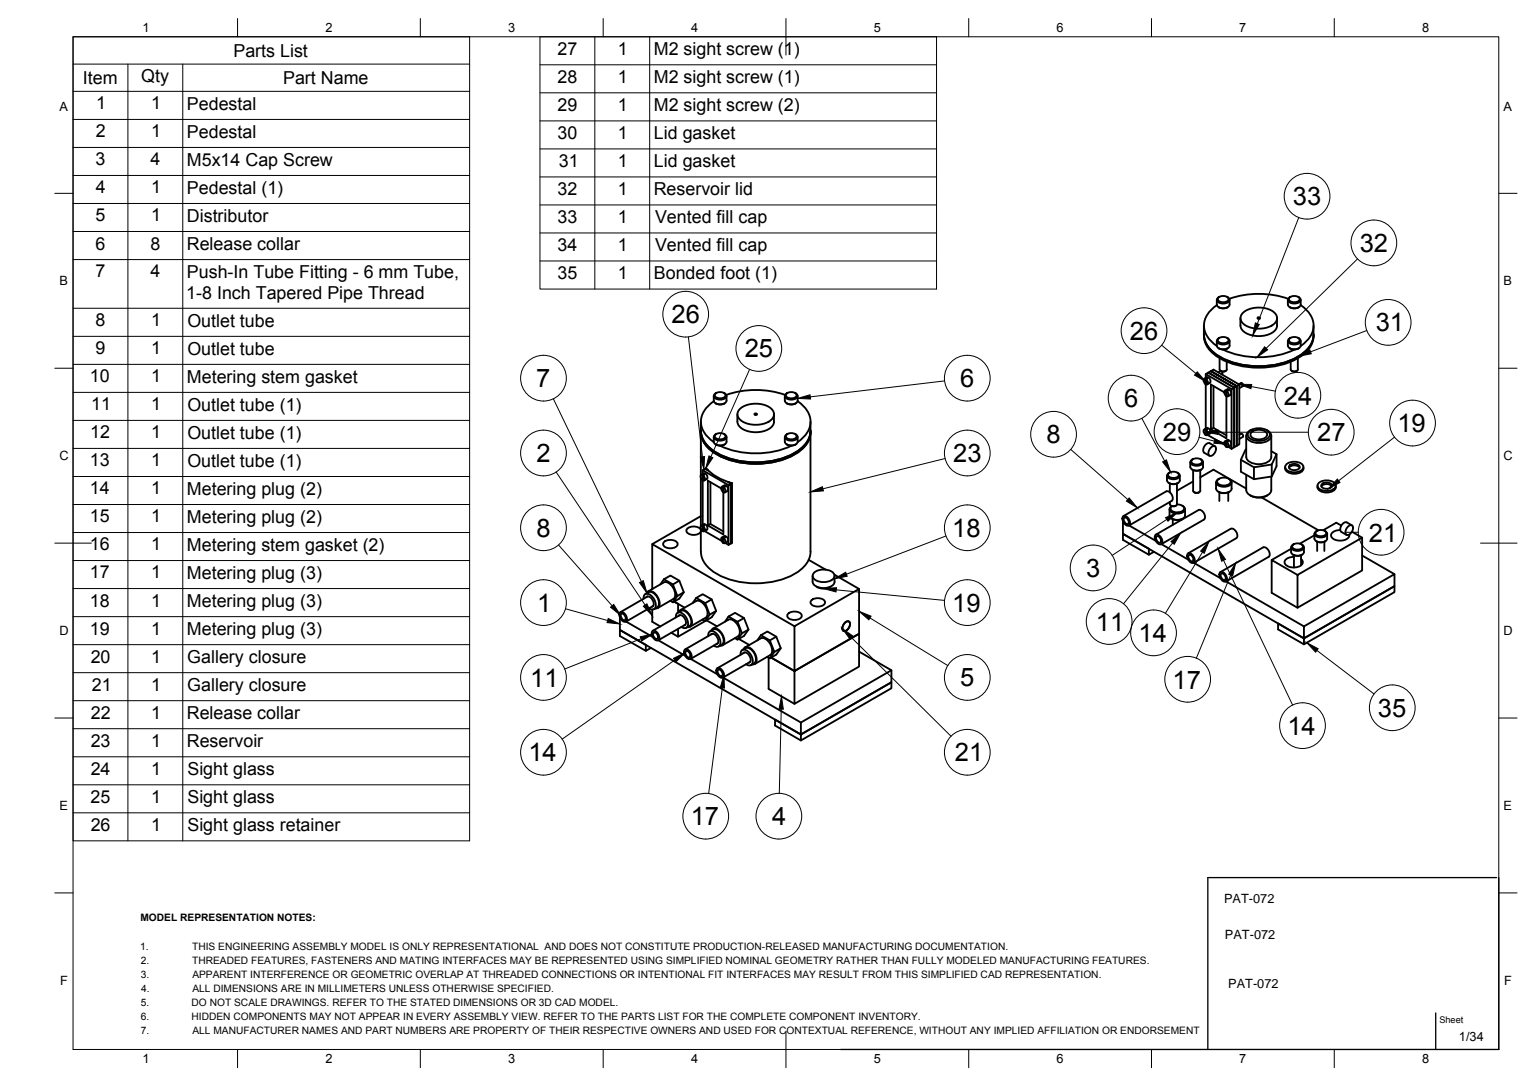
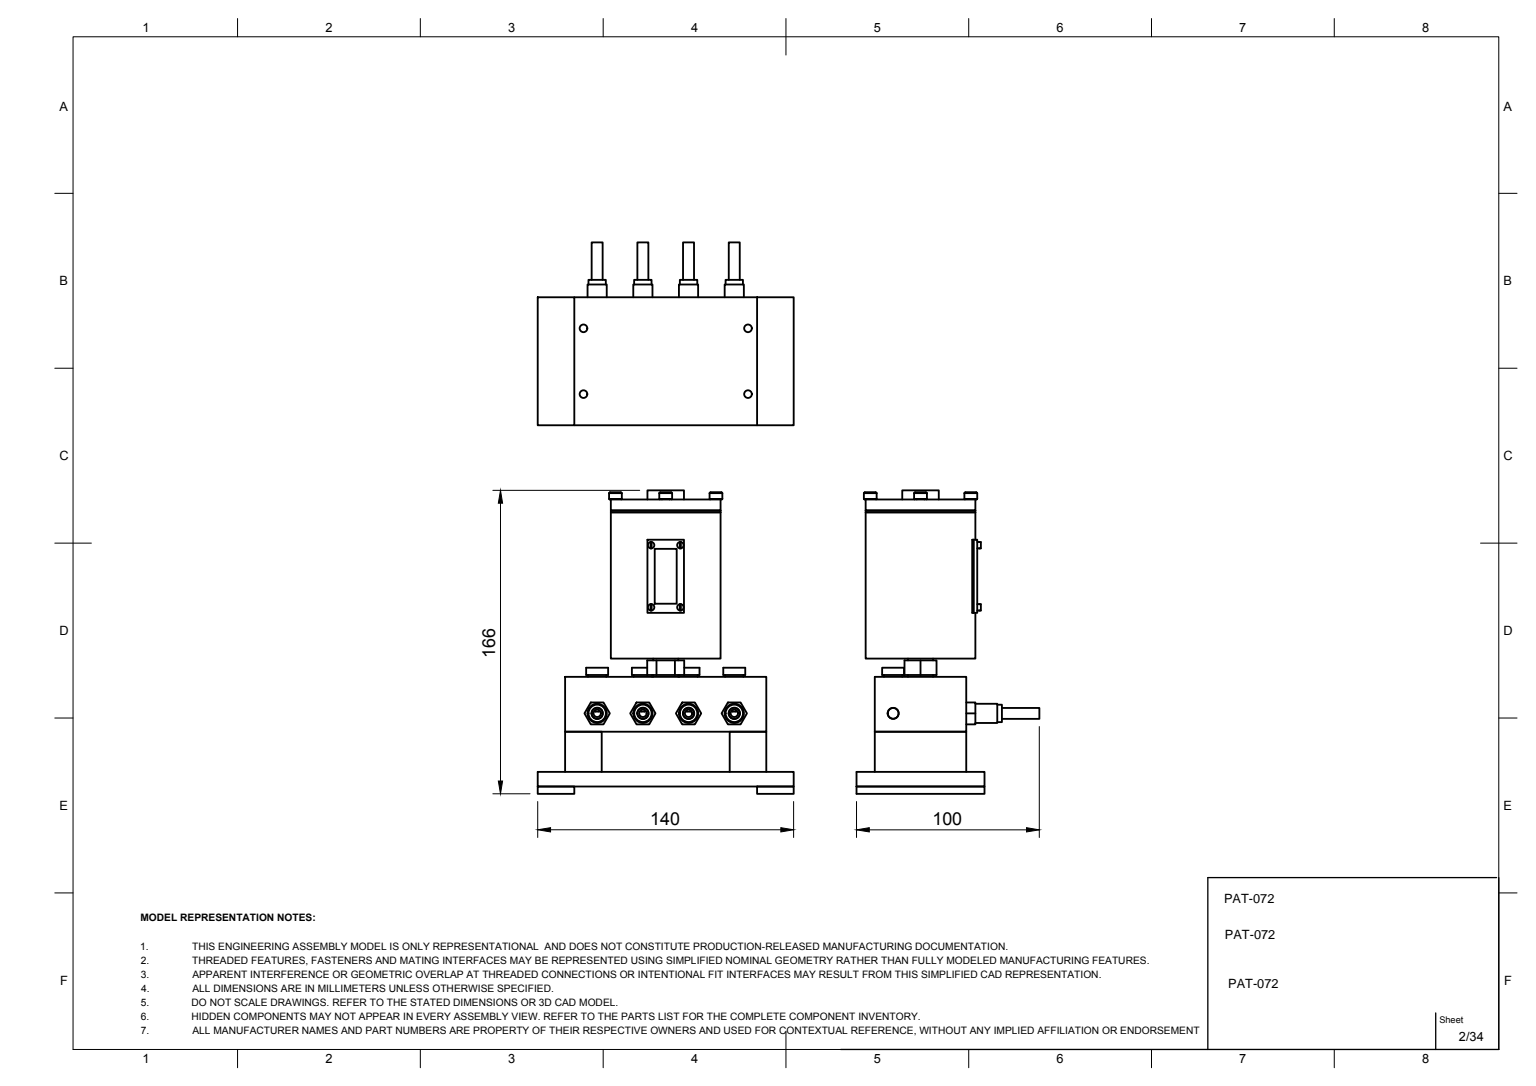
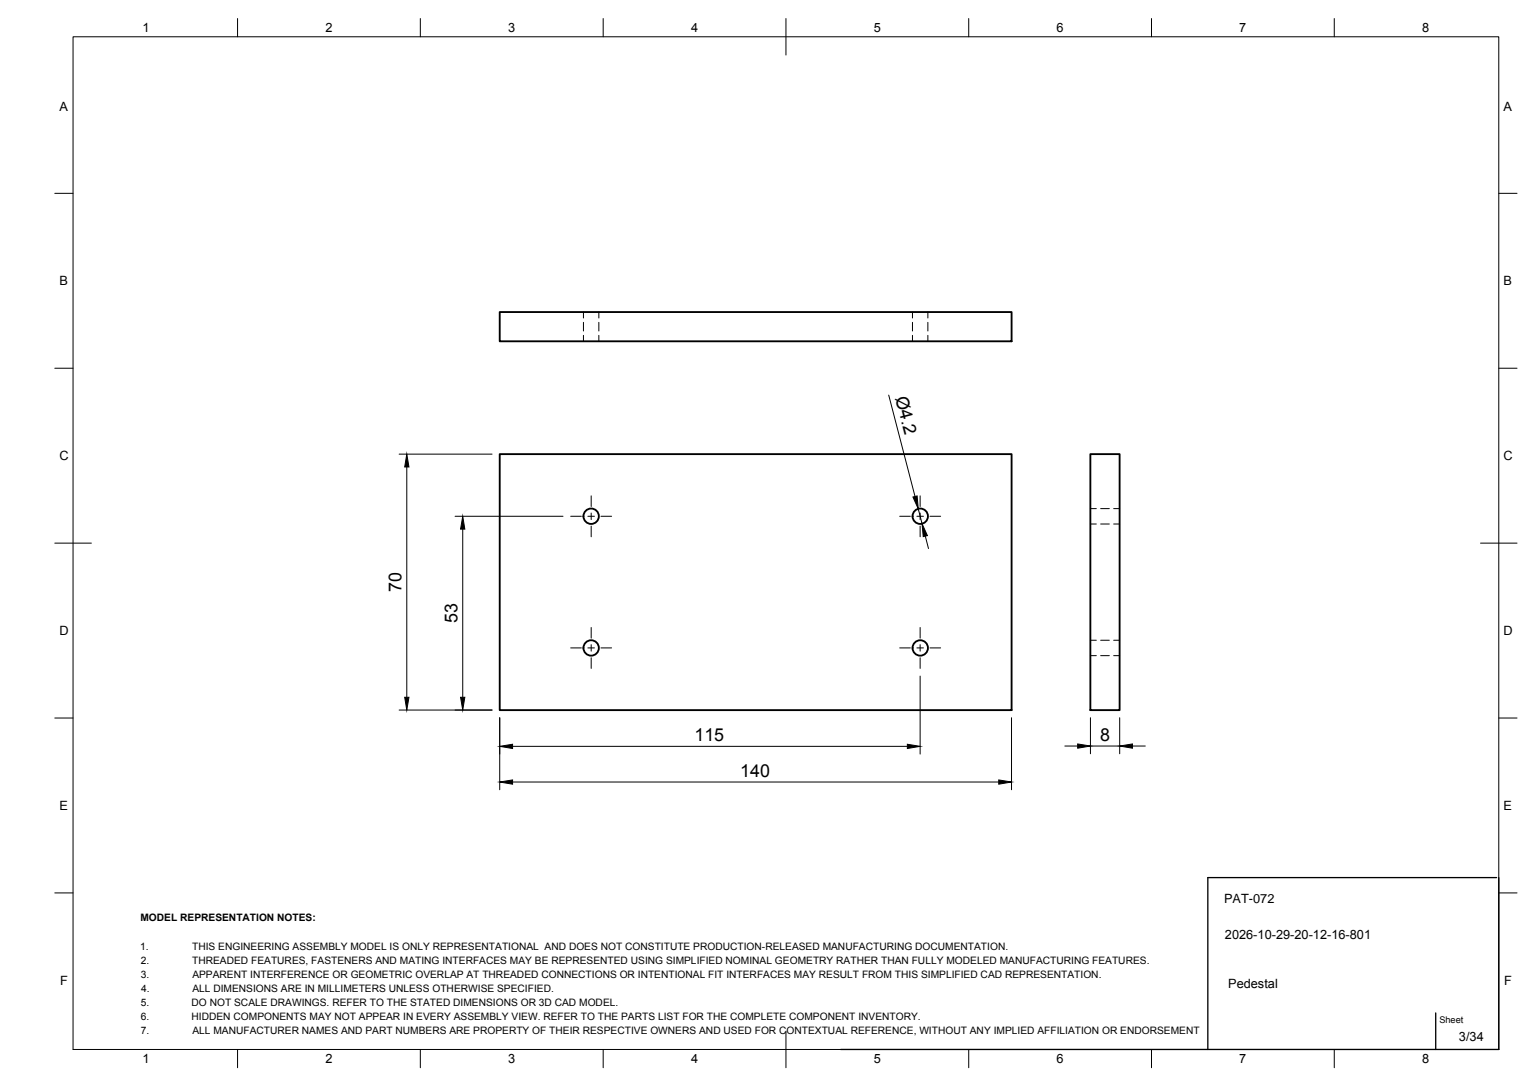
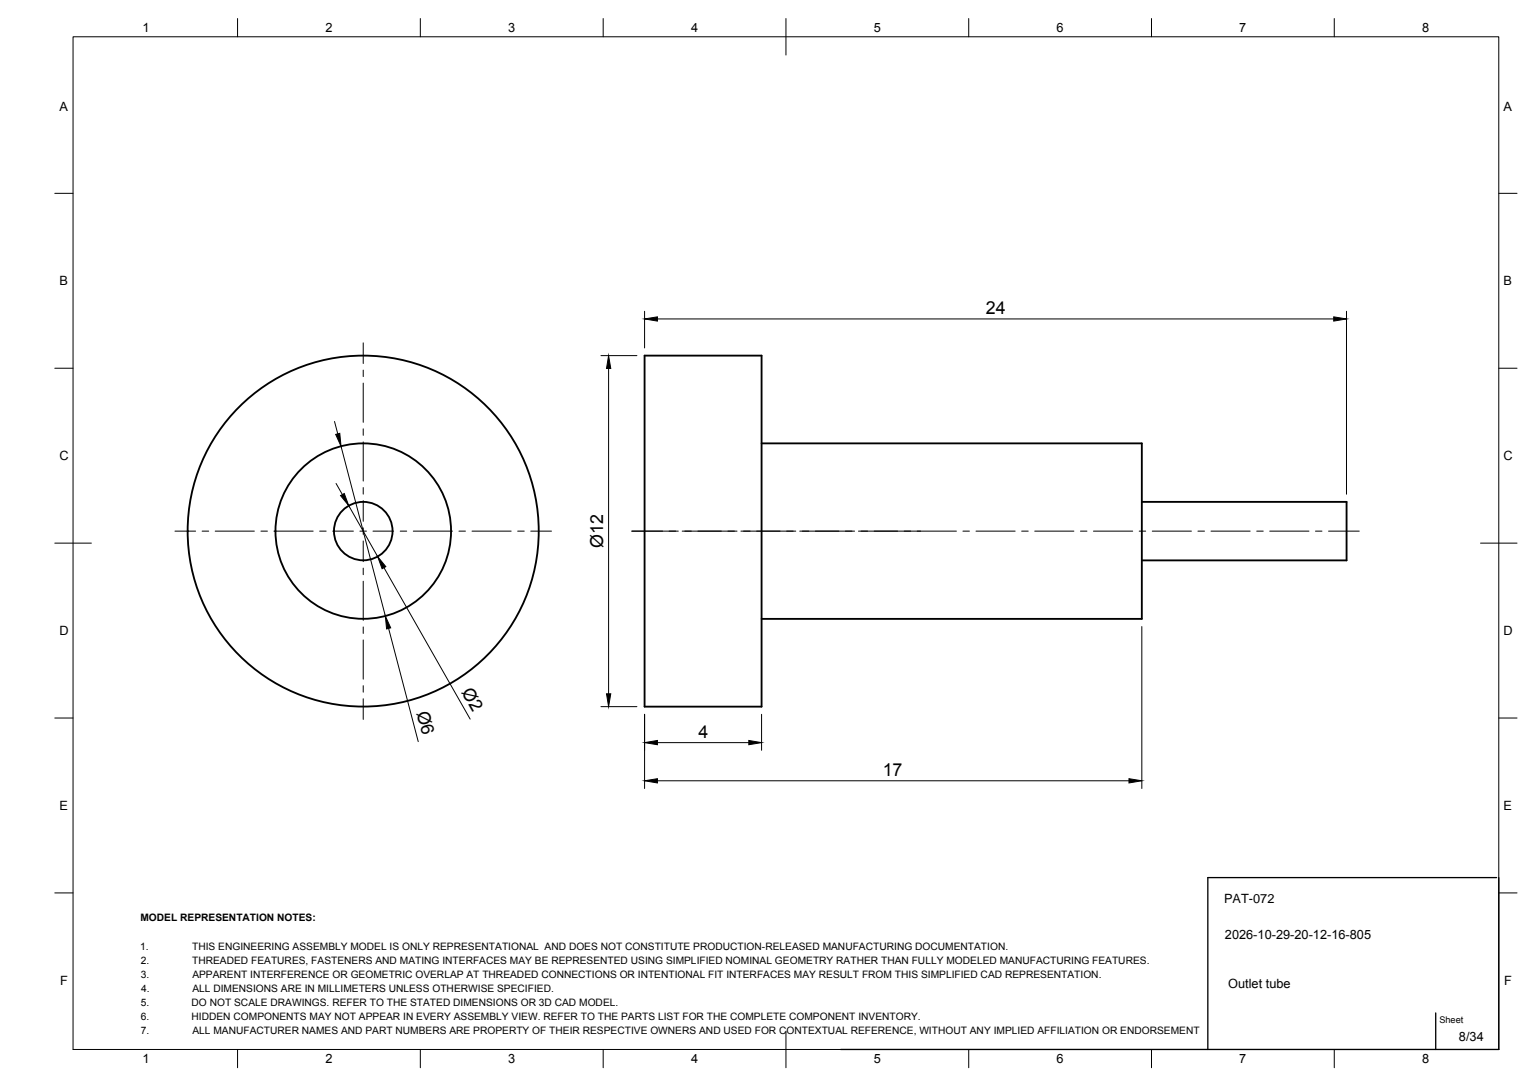
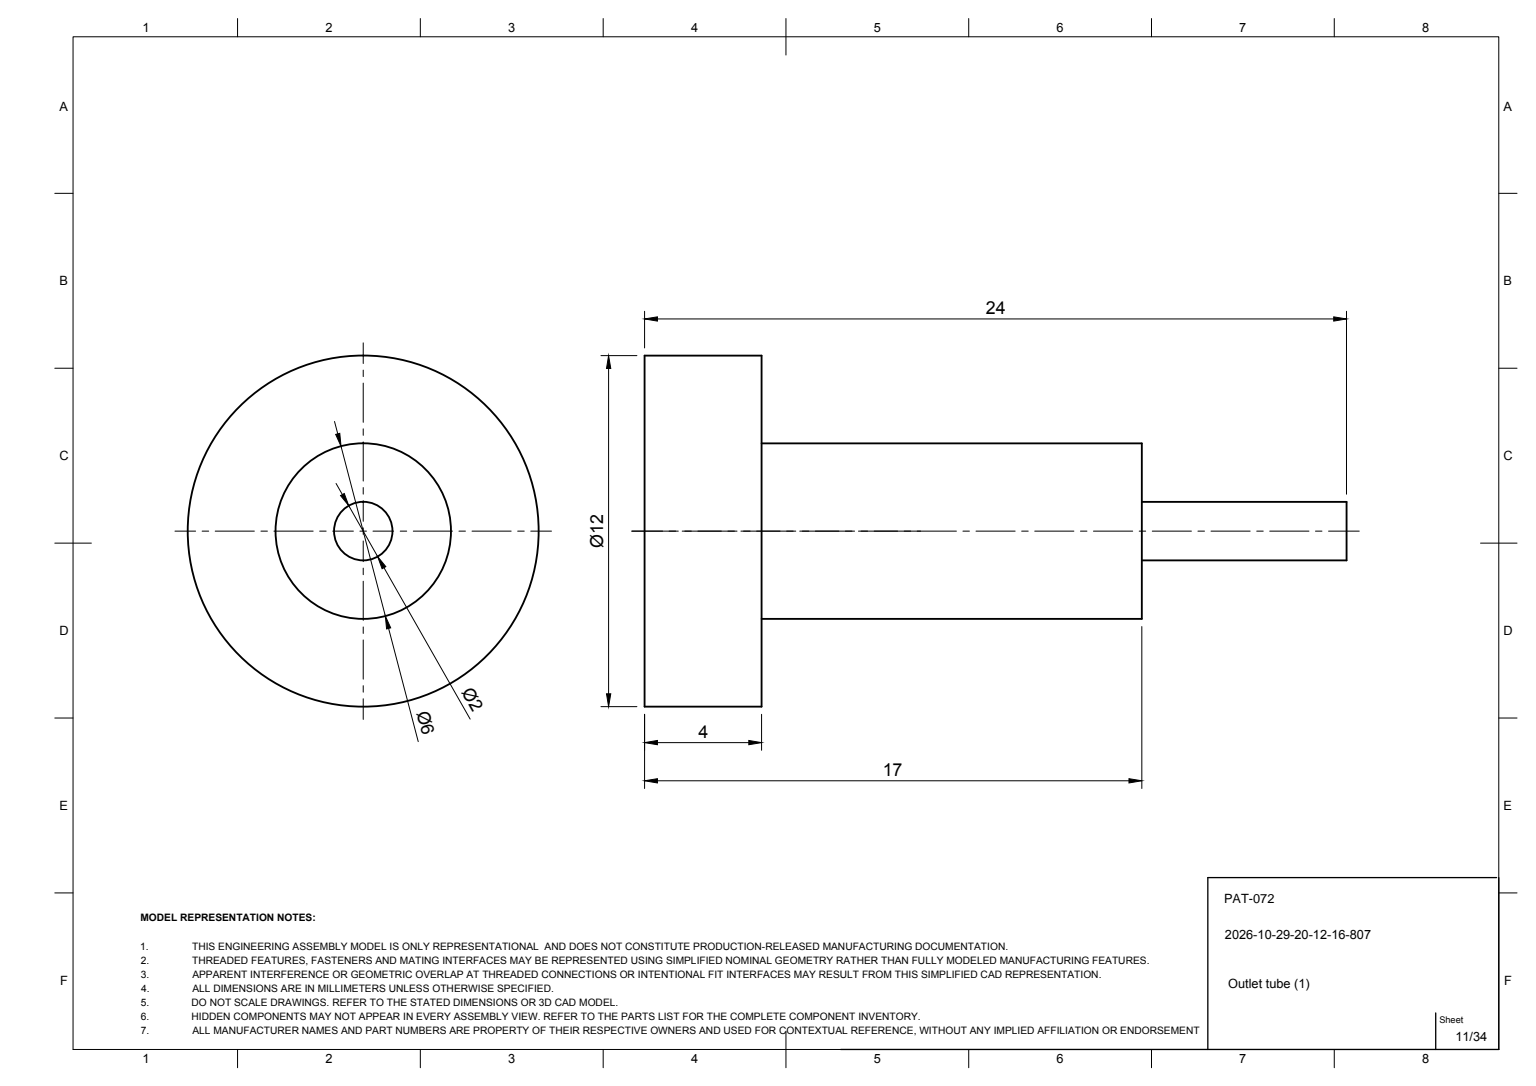
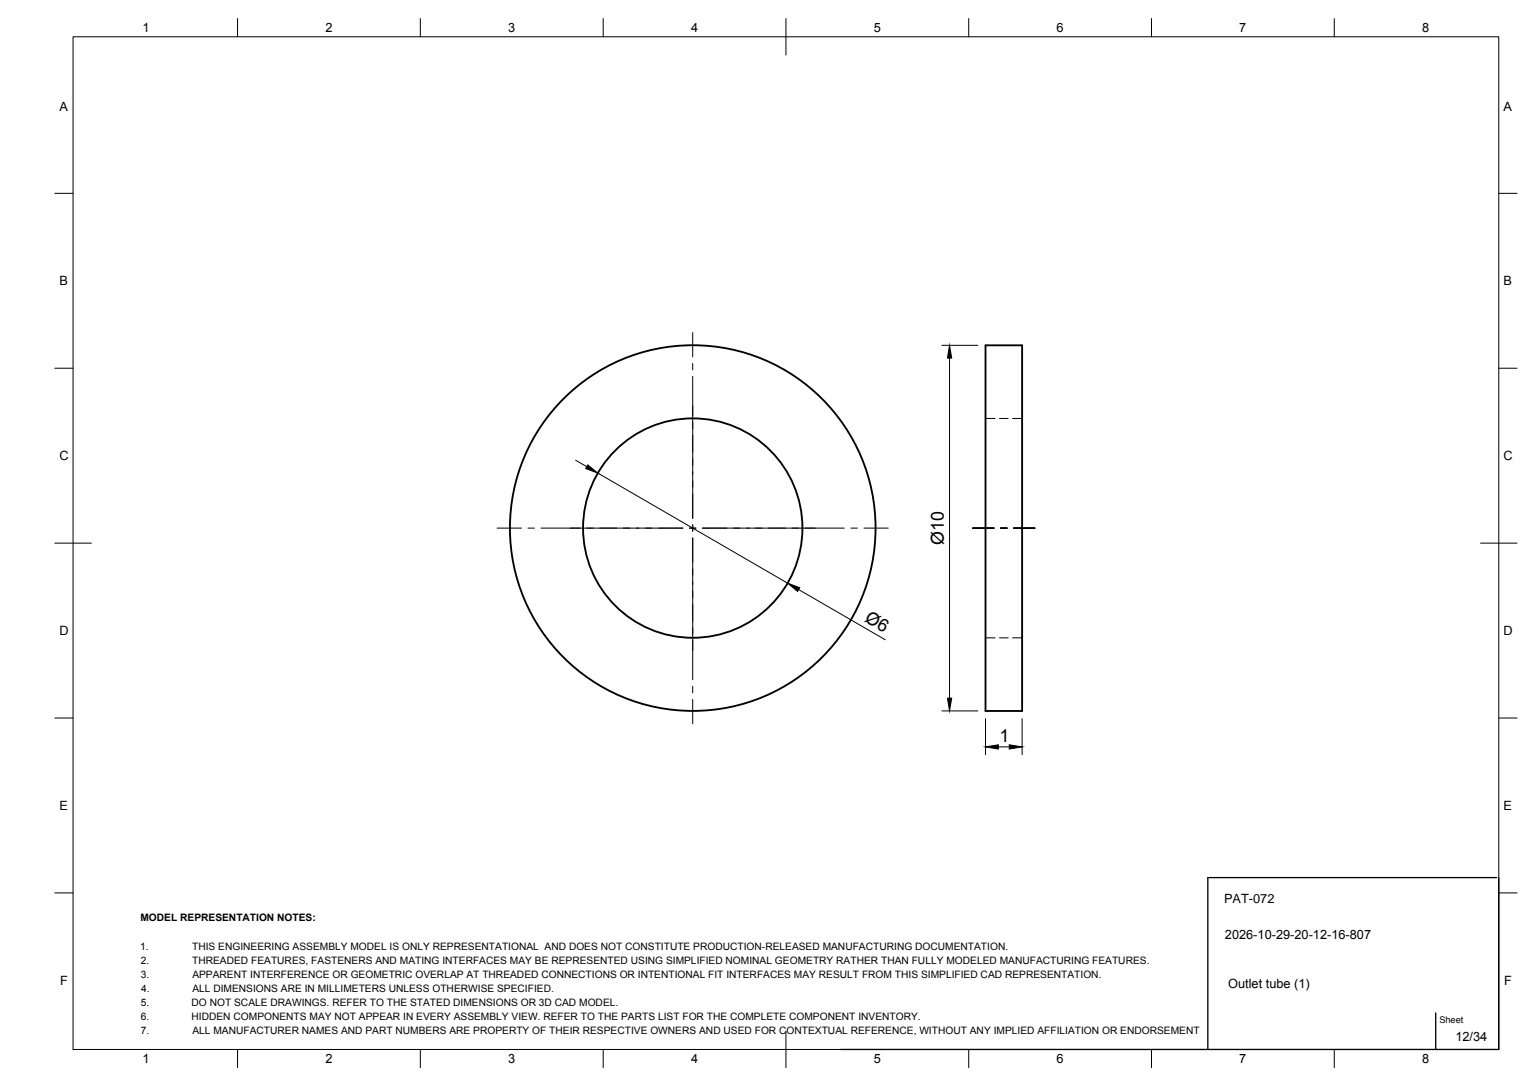
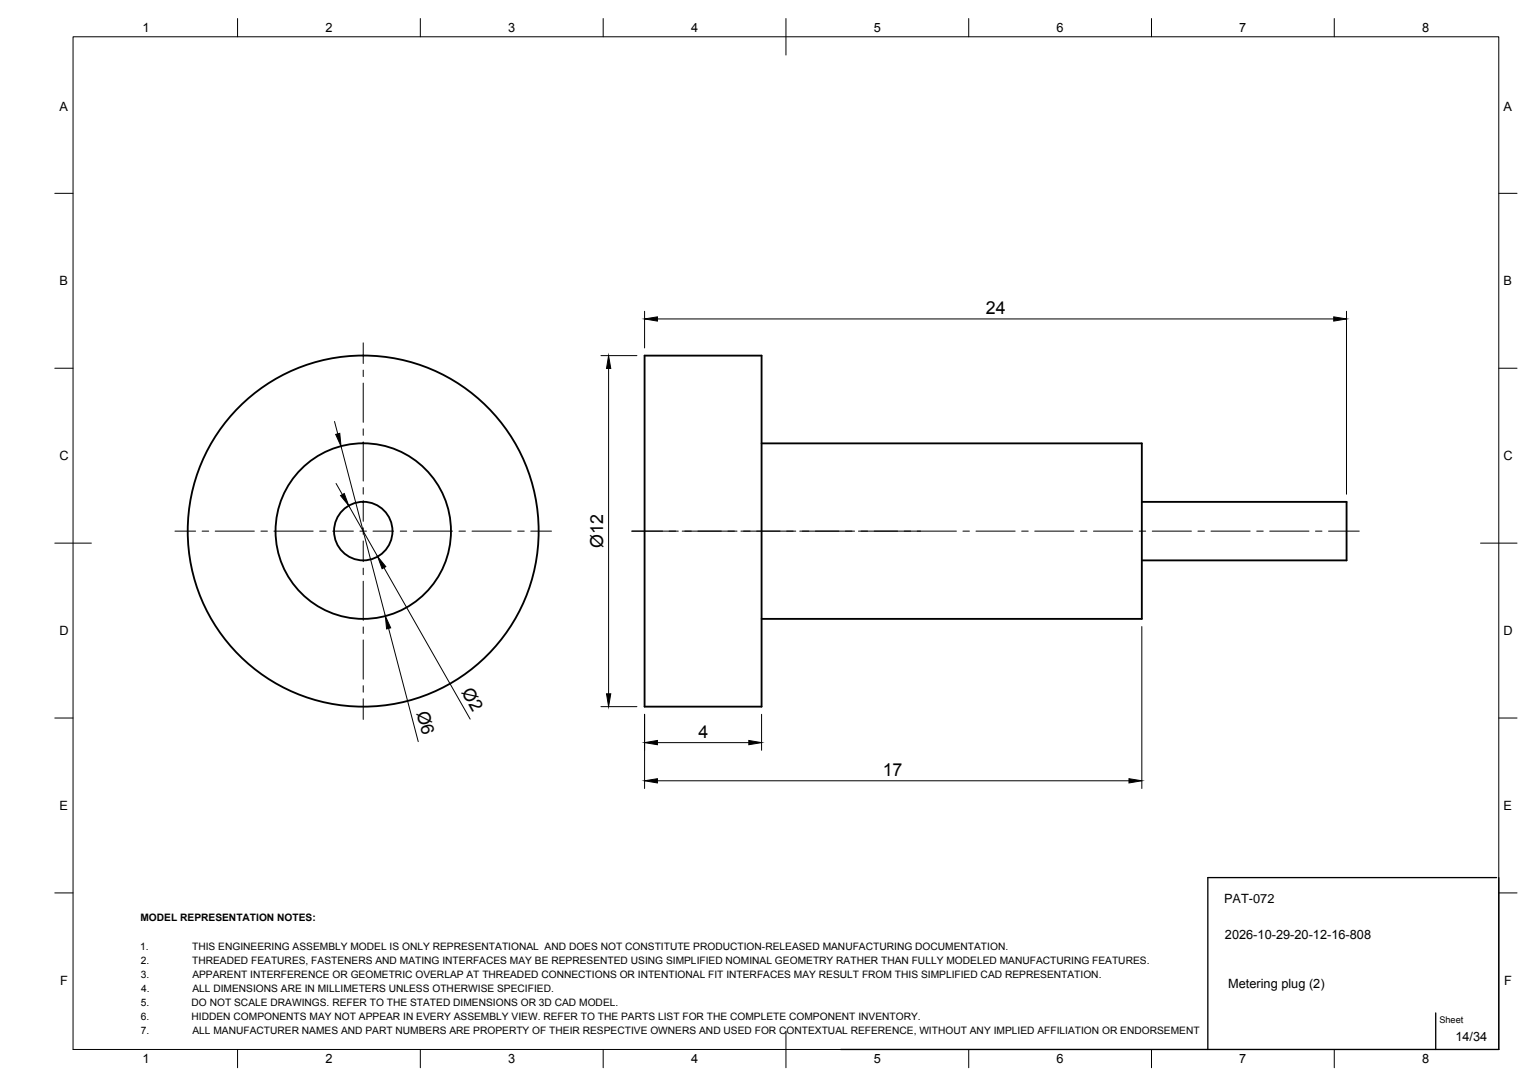
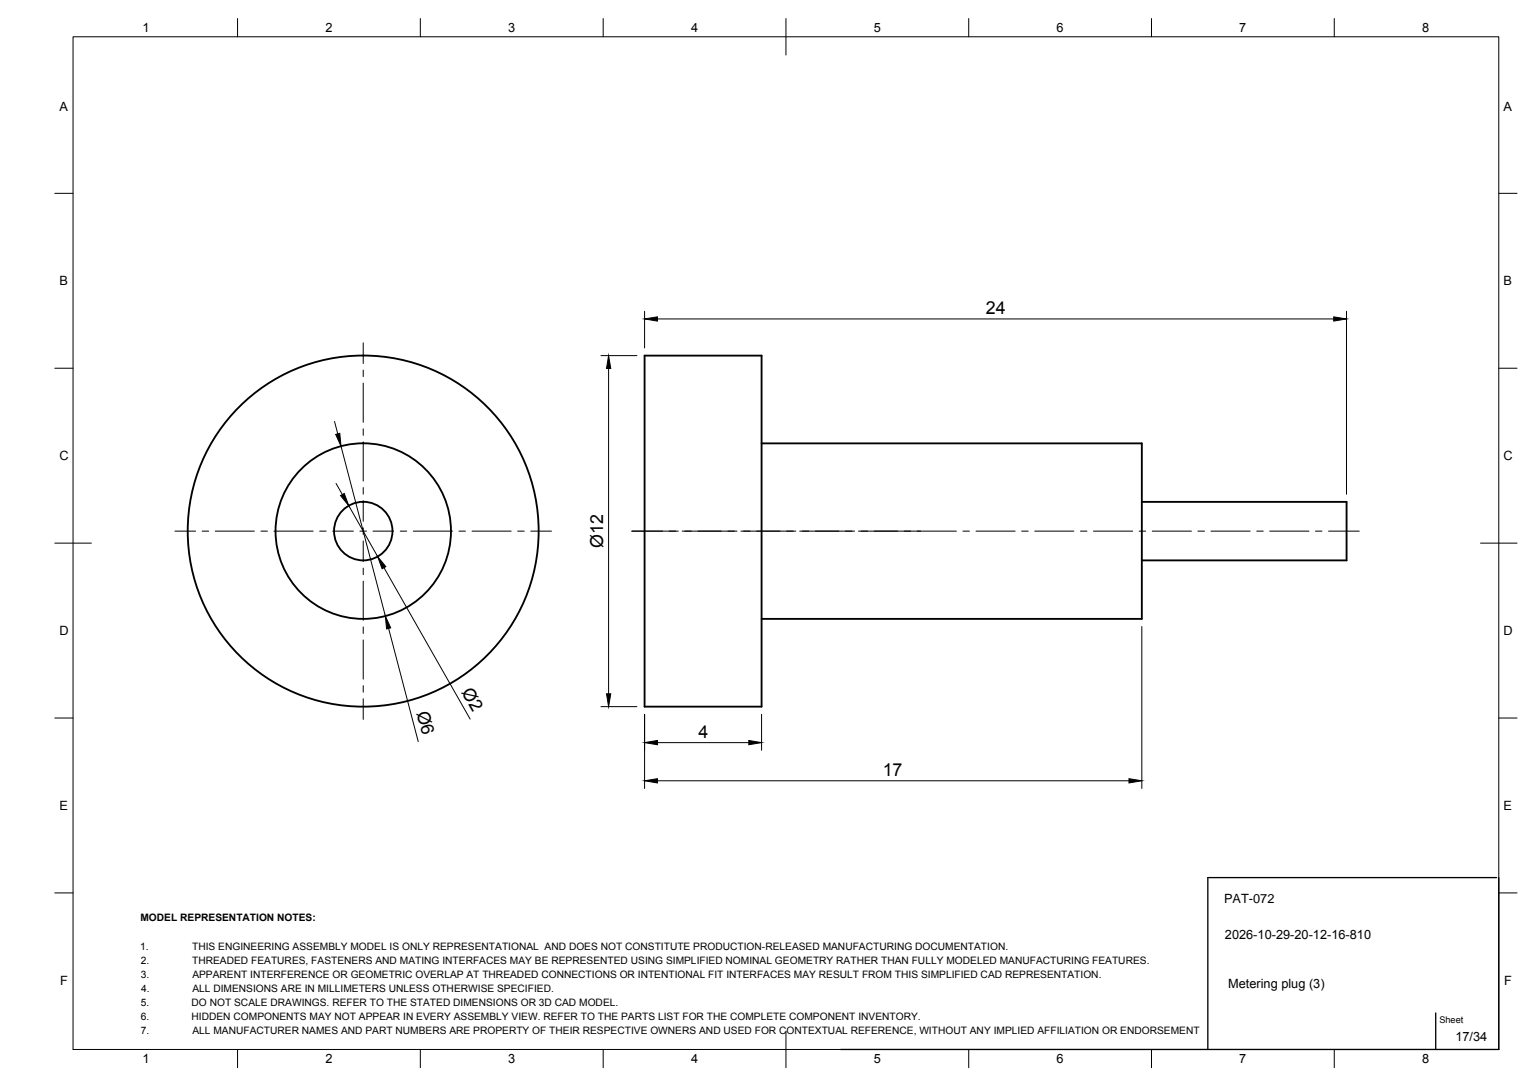
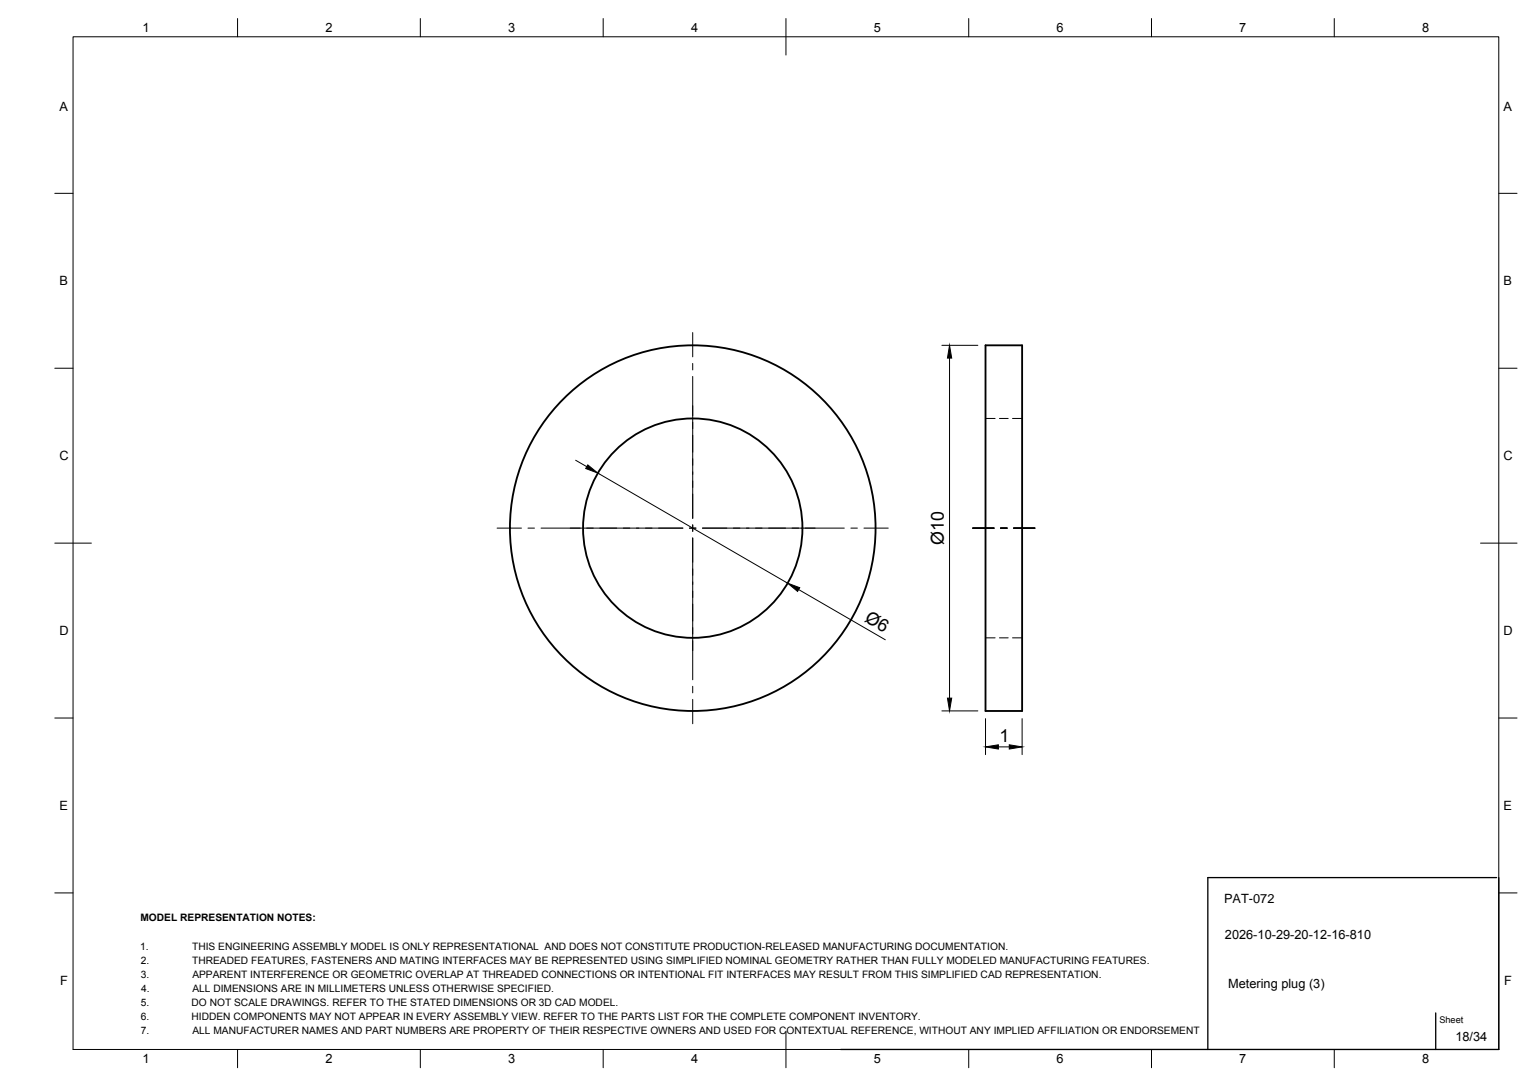
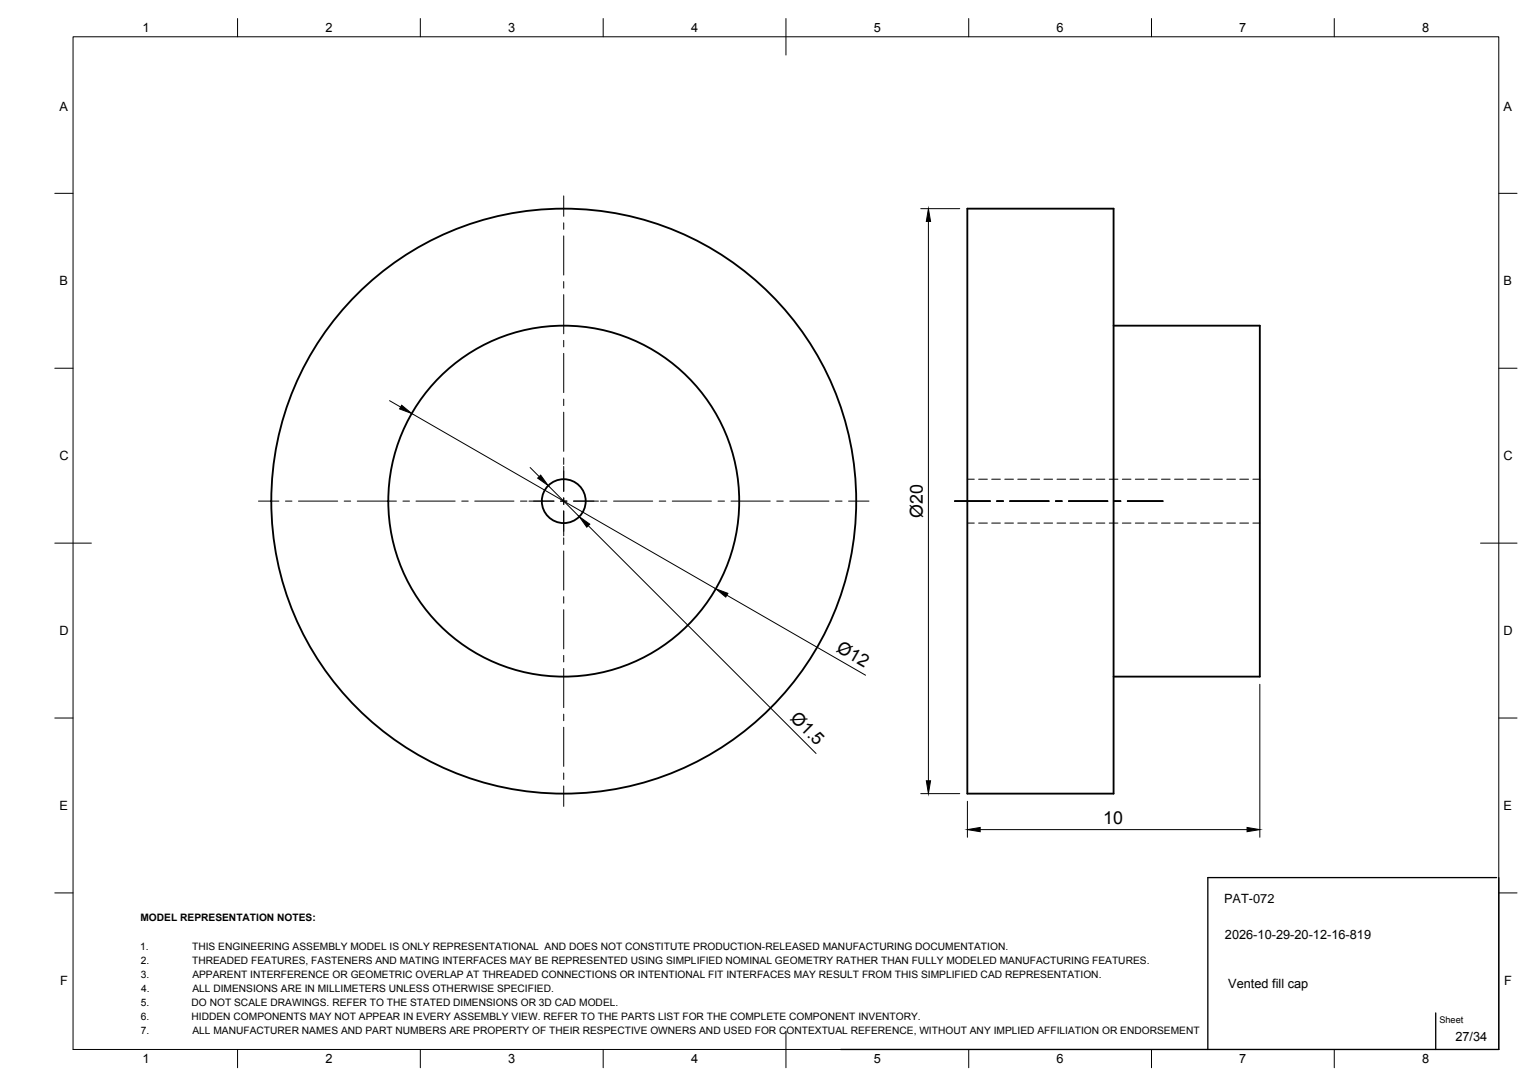
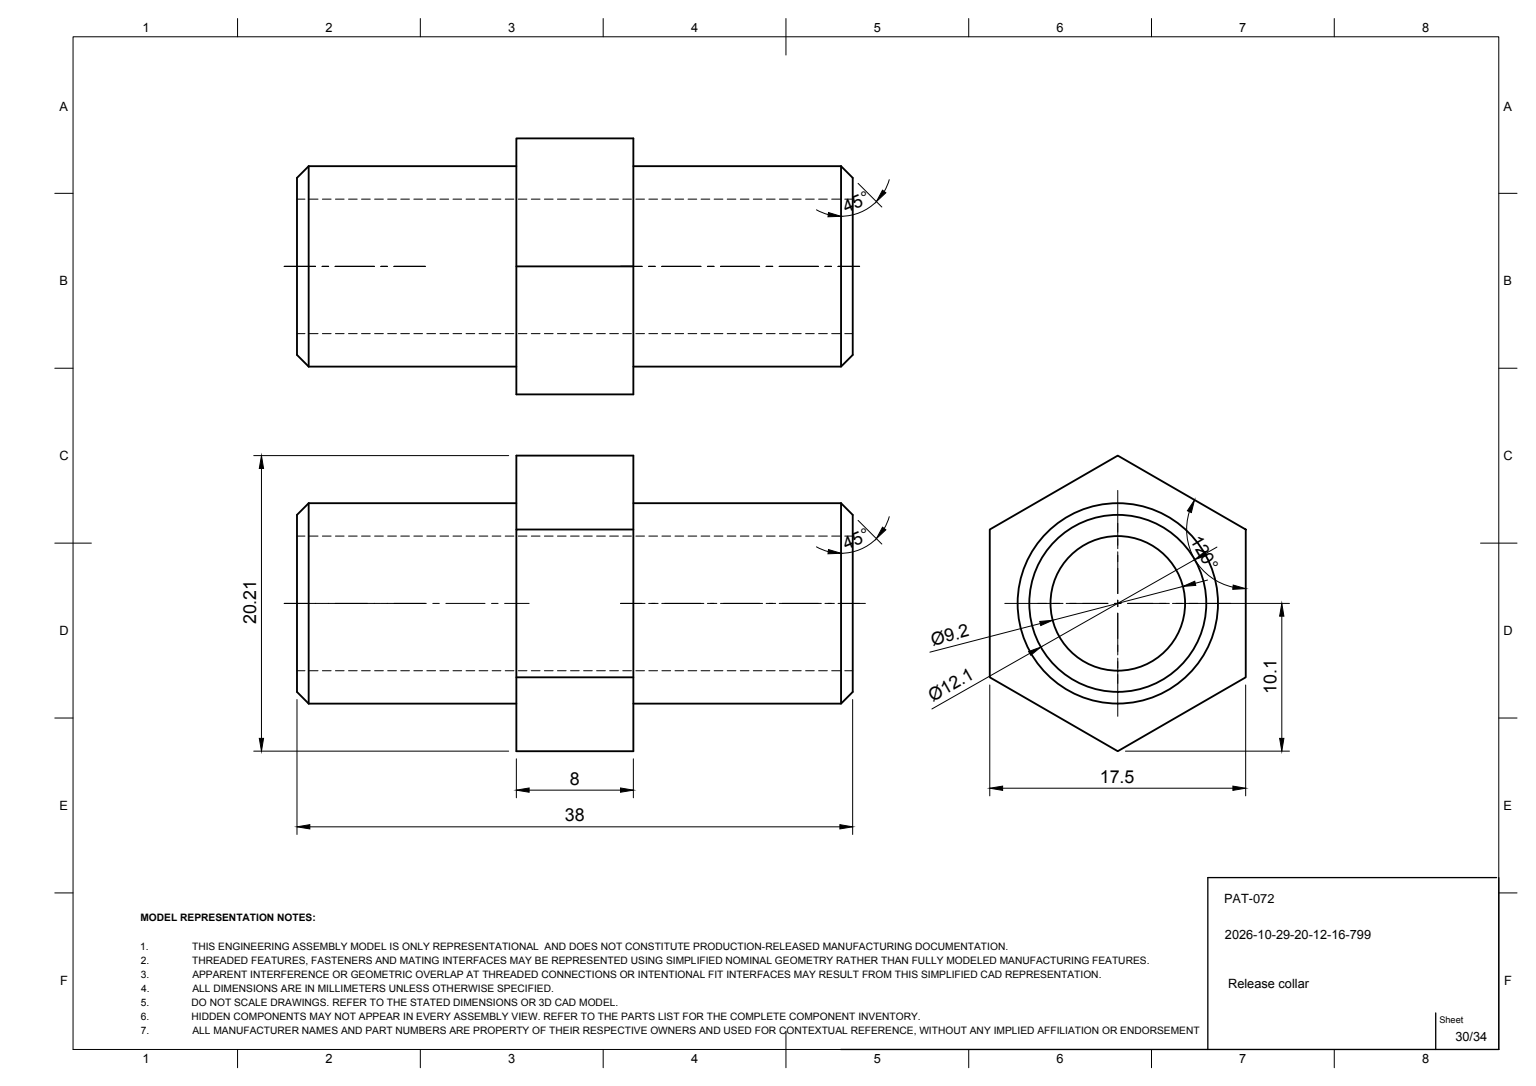
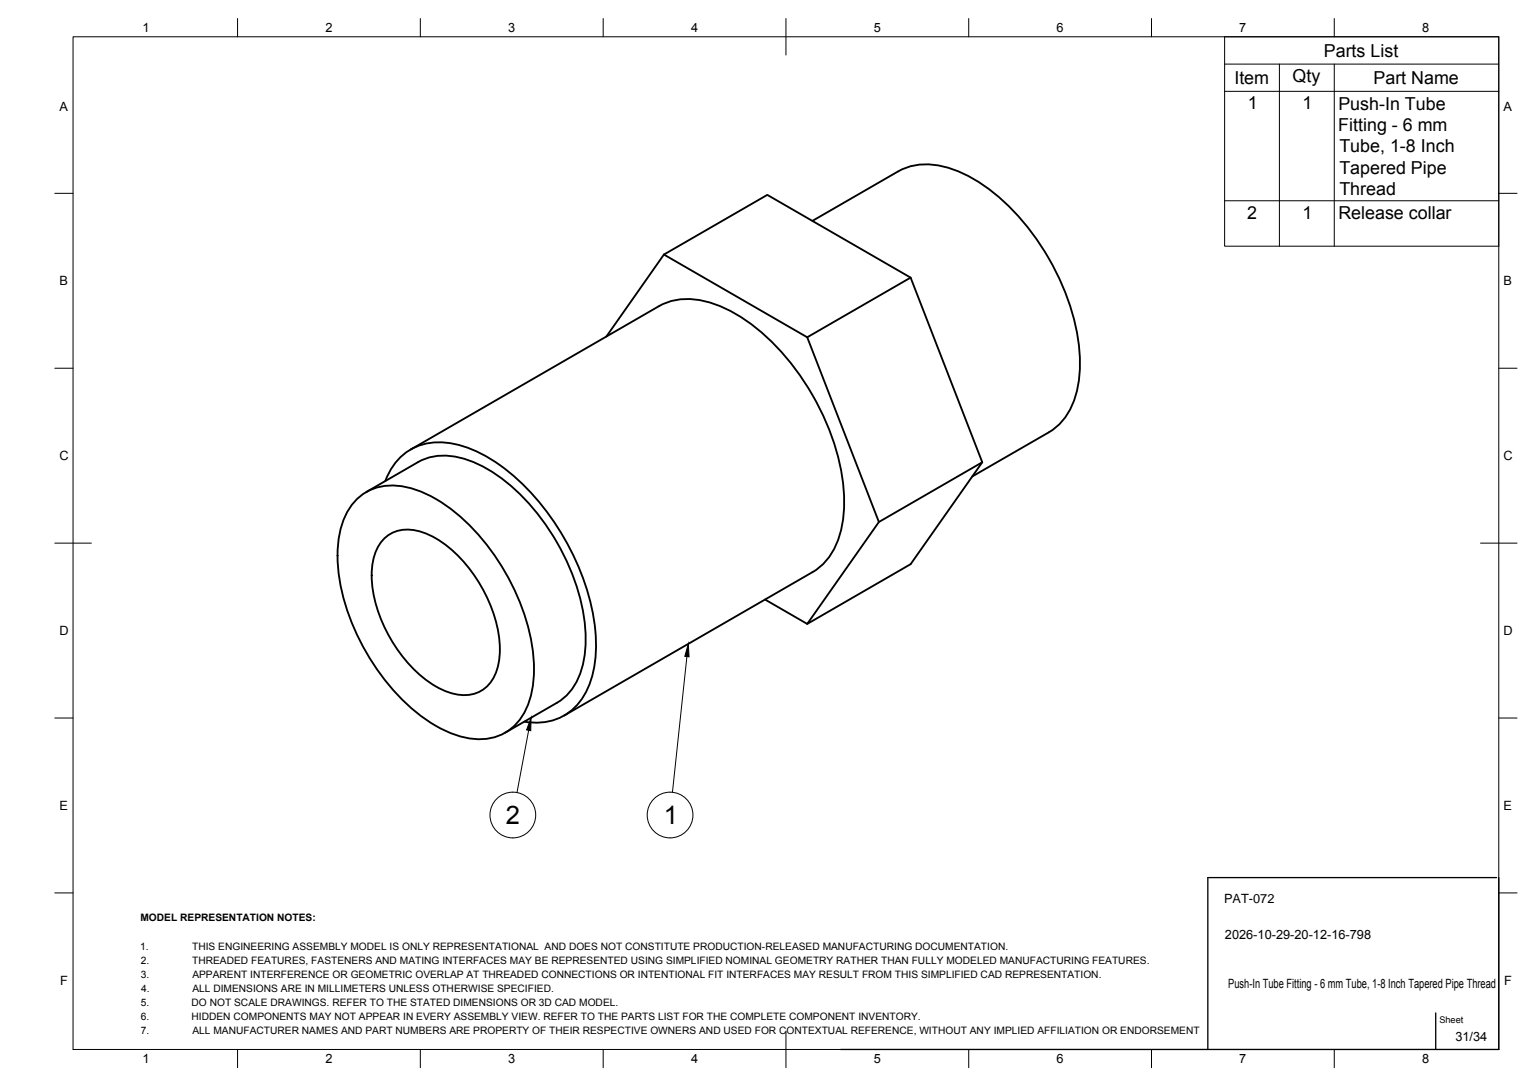
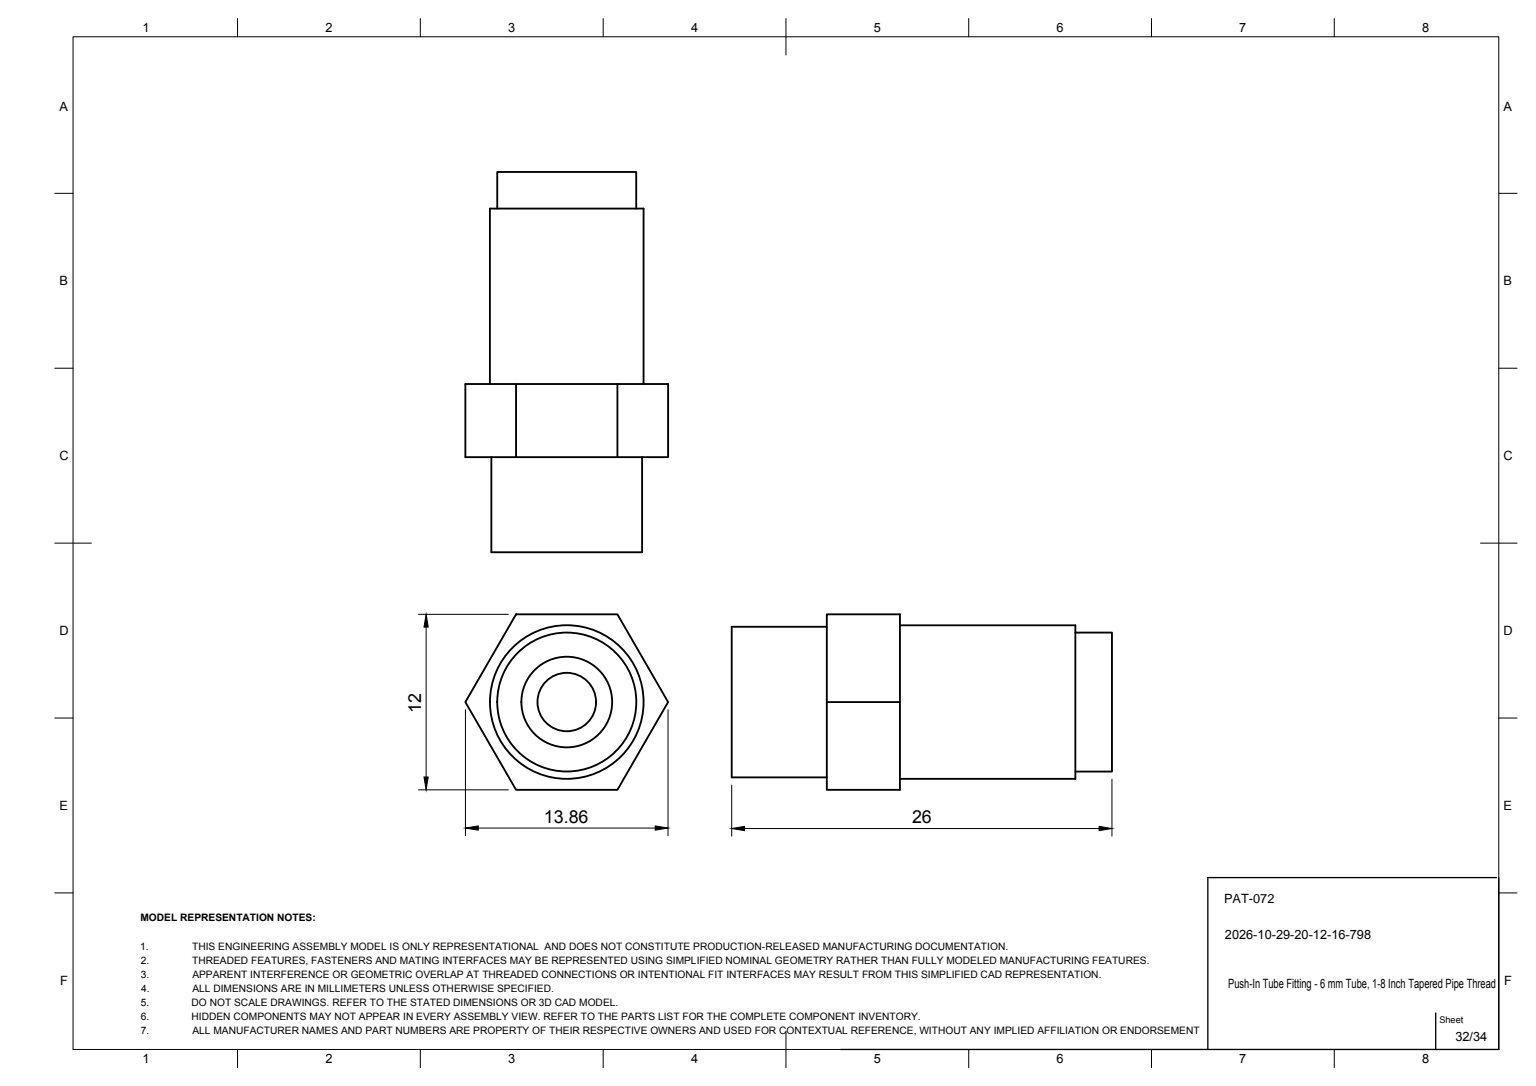
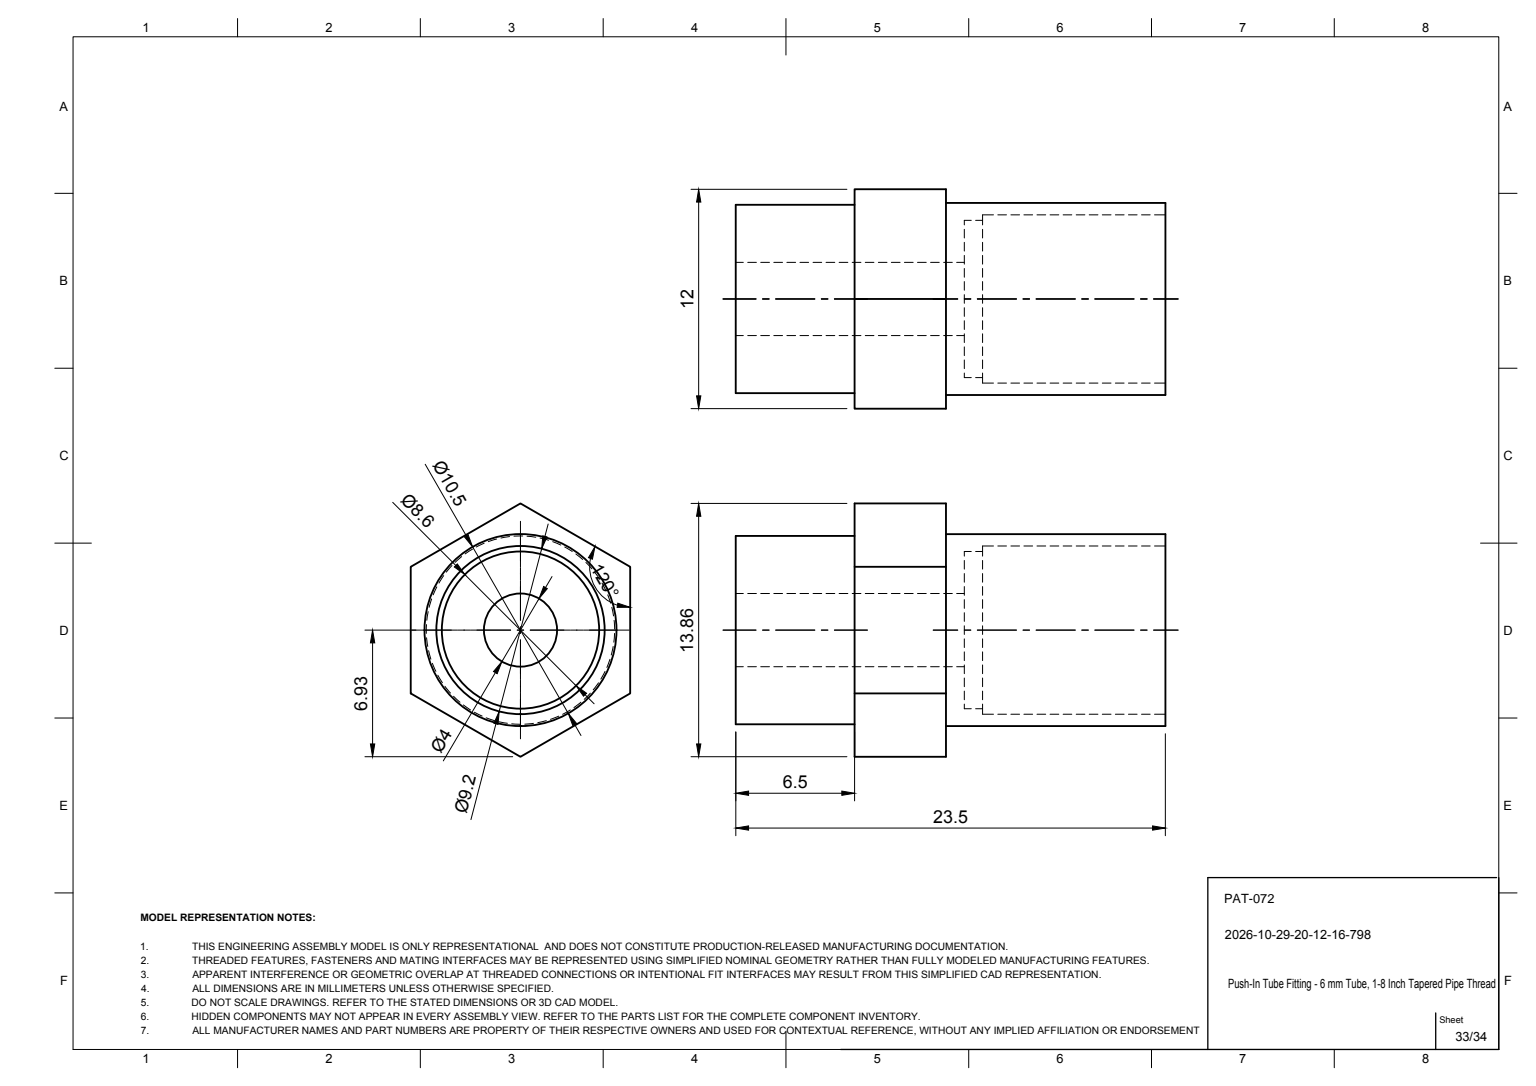
ISO-10303-21;
HEADER;
/* Generated by software containing ST-Developer
 * from STEP Tools, Inc. (www.steptools.com) 
 */

FILE_DESCRIPTION(
/* description */ ('PAT-072'),
/* implementation_level */ '2;1');

FILE_NAME(
/* name */ 'PAT-072',
/* time_stamp */ '2026-10-29T20:11:56-07:00',
/* author */ (''),
/* organization */ (''),
/* preprocessor_version */ 'ST-DEVELOPER v20.2',
/* originating_system */ 'Autodesk Translation Framework v15.17.0.0',
/* authorisation */ '');

FILE_SCHEMA (('AUTOMOTIVE_DESIGN { 1 0 10303 214 3 1 1 }'));
ENDSEC;

DATA;
#10=MECHANICAL_DESIGN_GEOMETRIC_PRESENTATION_REPRESENTATION('',(#332,#333,
#334,#335,#336,#337,#338,#339,#340,#341,#342,#343,#344,#345,#346,#347,#348,
#349,#350,#351,#352,#353,#354,#355,#356,#357,#358,#359,#360,#361,#362,#363,
#364,#365,#366,#367),#11432);
#11=ITEM_DEFINED_TRANSFORMATION($,$,#7118,#7159);
#12=ITEM_DEFINED_TRANSFORMATION($,$,#7146,#7160);
#13=ITEM_DEFINED_TRANSFORMATION($,$,#6503,#7211);
#14=ITEM_DEFINED_TRANSFORMATION($,$,#6522,#7212);
#15=ITEM_DEFINED_TRANSFORMATION($,$,#6547,#7213);
#16=ITEM_DEFINED_TRANSFORMATION($,$,#6572,#7214);
#17=ITEM_DEFINED_TRANSFORMATION($,$,#6692,#7215);
#18=ITEM_DEFINED_TRANSFORMATION($,$,#6701,#7216);
#19=ITEM_DEFINED_TRANSFORMATION($,$,#6715,#7217);
#20=ITEM_DEFINED_TRANSFORMATION($,$,#6724,#7218);
#21=ITEM_DEFINED_TRANSFORMATION($,$,#6733,#7219);
#22=ITEM_DEFINED_TRANSFORMATION($,$,#6747,#7220);
#23=ITEM_DEFINED_TRANSFORMATION($,$,#6756,#7221);
#24=ITEM_DEFINED_TRANSFORMATION($,$,#6765,#7222);
#25=ITEM_DEFINED_TRANSFORMATION($,$,#6779,#7223);
#26=ITEM_DEFINED_TRANSFORMATION($,$,#6788,#7224);
#27=ITEM_DEFINED_TRANSFORMATION($,$,#6797,#7225);
#28=ITEM_DEFINED_TRANSFORMATION($,$,#6811,#7226);
#29=ITEM_DEFINED_TRANSFORMATION($,$,#6820,#7227);
#30=ITEM_DEFINED_TRANSFORMATION($,$,#6826,#7228);
#31=ITEM_DEFINED_TRANSFORMATION($,$,#6832,#7229);
#32=ITEM_DEFINED_TRANSFORMATION($,$,#6887,#7230);
#33=ITEM_DEFINED_TRANSFORMATION($,$,#6910,#7231);
#34=ITEM_DEFINED_TRANSFORMATION($,$,#6929,#7232);
#35=ITEM_DEFINED_TRANSFORMATION($,$,#6952,#7233);
#36=ITEM_DEFINED_TRANSFORMATION($,$,#6970,#7234);
#37=ITEM_DEFINED_TRANSFORMATION($,$,#6988,#7235);
#38=ITEM_DEFINED_TRANSFORMATION($,$,#7006,#7236);
#39=ITEM_DEFINED_TRANSFORMATION($,$,#7024,#7237);
#40=ITEM_DEFINED_TRANSFORMATION($,$,#7045,#7238);
#41=ITEM_DEFINED_TRANSFORMATION($,$,#7066,#7239);
#42=ITEM_DEFINED_TRANSFORMATION($,$,#7079,#7240);
#43=ITEM_DEFINED_TRANSFORMATION($,$,#7086,#7241);
#44=ITEM_DEFINED_TRANSFORMATION($,$,#7093,#7242);
#45=ITEM_DEFINED_TRANSFORMATION($,$,#7093,#7243);
#46=ITEM_DEFINED_TRANSFORMATION($,$,#7093,#7244);
#47=ITEM_DEFINED_TRANSFORMATION($,$,#7093,#7245);
#48=ITEM_DEFINED_TRANSFORMATION($,$,#7185,#7246);
#49=ITEM_DEFINED_TRANSFORMATION($,$,#7185,#7247);
#50=ITEM_DEFINED_TRANSFORMATION($,$,#7185,#7248);
#51=ITEM_DEFINED_TRANSFORMATION($,$,#7185,#7249);
#52=ITEM_DEFINED_TRANSFORMATION($,$,#7117,#7250);
#53=ITEM_DEFINED_TRANSFORMATION($,$,#7117,#7251);
#54=ITEM_DEFINED_TRANSFORMATION($,$,#7117,#7252);
#55=ITEM_DEFINED_TRANSFORMATION($,$,#7117,#7253);
#56=ITEM_DEFINED_TRANSFORMATION($,$,#7161,#7254);
#57=ITEM_DEFINED_TRANSFORMATION($,$,#7185,#7255);
#58=ITEM_DEFINED_TRANSFORMATION($,$,#7185,#7256);
#59=ITEM_DEFINED_TRANSFORMATION($,$,#7185,#7257);
#60=ITEM_DEFINED_TRANSFORMATION($,$,#7185,#7258);
#61=(
REPRESENTATION_RELATIONSHIP($,$,#11597,#11596)
REPRESENTATION_RELATIONSHIP_WITH_TRANSFORMATION(#11)
SHAPE_REPRESENTATION_RELATIONSHIP()
);
#62=(
REPRESENTATION_RELATIONSHIP($,$,#11598,#11596)
REPRESENTATION_RELATIONSHIP_WITH_TRANSFORMATION(#12)
SHAPE_REPRESENTATION_RELATIONSHIP()
);
#63=(
REPRESENTATION_RELATIONSHIP($,$,#11564,#11563)
REPRESENTATION_RELATIONSHIP_WITH_TRANSFORMATION(#13)
SHAPE_REPRESENTATION_RELATIONSHIP()
);
#64=(
REPRESENTATION_RELATIONSHIP($,$,#11565,#11563)
REPRESENTATION_RELATIONSHIP_WITH_TRANSFORMATION(#14)
SHAPE_REPRESENTATION_RELATIONSHIP()
);
#65=(
REPRESENTATION_RELATIONSHIP($,$,#11566,#11563)
REPRESENTATION_RELATIONSHIP_WITH_TRANSFORMATION(#15)
SHAPE_REPRESENTATION_RELATIONSHIP()
);
#66=(
REPRESENTATION_RELATIONSHIP($,$,#11567,#11563)
REPRESENTATION_RELATIONSHIP_WITH_TRANSFORMATION(#16)
SHAPE_REPRESENTATION_RELATIONSHIP()
);
#67=(
REPRESENTATION_RELATIONSHIP($,$,#11568,#11563)
REPRESENTATION_RELATIONSHIP_WITH_TRANSFORMATION(#17)
SHAPE_REPRESENTATION_RELATIONSHIP()
);
#68=(
REPRESENTATION_RELATIONSHIP($,$,#11569,#11563)
REPRESENTATION_RELATIONSHIP_WITH_TRANSFORMATION(#18)
SHAPE_REPRESENTATION_RELATIONSHIP()
);
#69=(
REPRESENTATION_RELATIONSHIP($,$,#11570,#11563)
REPRESENTATION_RELATIONSHIP_WITH_TRANSFORMATION(#19)
SHAPE_REPRESENTATION_RELATIONSHIP()
);
#70=(
REPRESENTATION_RELATIONSHIP($,$,#11571,#11563)
REPRESENTATION_RELATIONSHIP_WITH_TRANSFORMATION(#20)
SHAPE_REPRESENTATION_RELATIONSHIP()
);
#71=(
REPRESENTATION_RELATIONSHIP($,$,#11572,#11563)
REPRESENTATION_RELATIONSHIP_WITH_TRANSFORMATION(#21)
SHAPE_REPRESENTATION_RELATIONSHIP()
);
#72=(
REPRESENTATION_RELATIONSHIP($,$,#11573,#11563)
REPRESENTATION_RELATIONSHIP_WITH_TRANSFORMATION(#22)
SHAPE_REPRESENTATION_RELATIONSHIP()
);
#73=(
REPRESENTATION_RELATIONSHIP($,$,#11574,#11563)
REPRESENTATION_RELATIONSHIP_WITH_TRANSFORMATION(#23)
SHAPE_REPRESENTATION_RELATIONSHIP()
);
#74=(
REPRESENTATION_RELATIONSHIP($,$,#11575,#11563)
REPRESENTATION_RELATIONSHIP_WITH_TRANSFORMATION(#24)
SHAPE_REPRESENTATION_RELATIONSHIP()
);
#75=(
REPRESENTATION_RELATIONSHIP($,$,#11576,#11563)
REPRESENTATION_RELATIONSHIP_WITH_TRANSFORMATION(#25)
SHAPE_REPRESENTATION_RELATIONSHIP()
);
#76=(
REPRESENTATION_RELATIONSHIP($,$,#11577,#11563)
REPRESENTATION_RELATIONSHIP_WITH_TRANSFORMATION(#26)
SHAPE_REPRESENTATION_RELATIONSHIP()
);
#77=(
REPRESENTATION_RELATIONSHIP($,$,#11578,#11563)
REPRESENTATION_RELATIONSHIP_WITH_TRANSFORMATION(#27)
SHAPE_REPRESENTATION_RELATIONSHIP()
);
#78=(
REPRESENTATION_RELATIONSHIP($,$,#11579,#11563)
REPRESENTATION_RELATIONSHIP_WITH_TRANSFORMATION(#28)
SHAPE_REPRESENTATION_RELATIONSHIP()
);
#79=(
REPRESENTATION_RELATIONSHIP($,$,#11580,#11563)
REPRESENTATION_RELATIONSHIP_WITH_TRANSFORMATION(#29)
SHAPE_REPRESENTATION_RELATIONSHIP()
);
#80=(
REPRESENTATION_RELATIONSHIP($,$,#11581,#11563)
REPRESENTATION_RELATIONSHIP_WITH_TRANSFORMATION(#30)
SHAPE_REPRESENTATION_RELATIONSHIP()
);
#81=(
REPRESENTATION_RELATIONSHIP($,$,#11582,#11563)
REPRESENTATION_RELATIONSHIP_WITH_TRANSFORMATION(#31)
SHAPE_REPRESENTATION_RELATIONSHIP()
);
#82=(
REPRESENTATION_RELATIONSHIP($,$,#11583,#11563)
REPRESENTATION_RELATIONSHIP_WITH_TRANSFORMATION(#32)
SHAPE_REPRESENTATION_RELATIONSHIP()
);
#83=(
REPRESENTATION_RELATIONSHIP($,$,#11584,#11563)
REPRESENTATION_RELATIONSHIP_WITH_TRANSFORMATION(#33)
SHAPE_REPRESENTATION_RELATIONSHIP()
);
#84=(
REPRESENTATION_RELATIONSHIP($,$,#11585,#11563)
REPRESENTATION_RELATIONSHIP_WITH_TRANSFORMATION(#34)
SHAPE_REPRESENTATION_RELATIONSHIP()
);
#85=(
REPRESENTATION_RELATIONSHIP($,$,#11586,#11563)
REPRESENTATION_RELATIONSHIP_WITH_TRANSFORMATION(#35)
SHAPE_REPRESENTATION_RELATIONSHIP()
);
#86=(
REPRESENTATION_RELATIONSHIP($,$,#11587,#11563)
REPRESENTATION_RELATIONSHIP_WITH_TRANSFORMATION(#36)
SHAPE_REPRESENTATION_RELATIONSHIP()
);
#87=(
REPRESENTATION_RELATIONSHIP($,$,#11588,#11563)
REPRESENTATION_RELATIONSHIP_WITH_TRANSFORMATION(#37)
SHAPE_REPRESENTATION_RELATIONSHIP()
);
#88=(
REPRESENTATION_RELATIONSHIP($,$,#11589,#11563)
REPRESENTATION_RELATIONSHIP_WITH_TRANSFORMATION(#38)
SHAPE_REPRESENTATION_RELATIONSHIP()
);
#89=(
REPRESENTATION_RELATIONSHIP($,$,#11590,#11563)
REPRESENTATION_RELATIONSHIP_WITH_TRANSFORMATION(#39)
SHAPE_REPRESENTATION_RELATIONSHIP()
);
#90=(
REPRESENTATION_RELATIONSHIP($,$,#11591,#11563)
REPRESENTATION_RELATIONSHIP_WITH_TRANSFORMATION(#40)
SHAPE_REPRESENTATION_RELATIONSHIP()
);
#91=(
REPRESENTATION_RELATIONSHIP($,$,#11592,#11563)
REPRESENTATION_RELATIONSHIP_WITH_TRANSFORMATION(#41)
SHAPE_REPRESENTATION_RELATIONSHIP()
);
#92=(
REPRESENTATION_RELATIONSHIP($,$,#11593,#11563)
REPRESENTATION_RELATIONSHIP_WITH_TRANSFORMATION(#42)
SHAPE_REPRESENTATION_RELATIONSHIP()
);
#93=(
REPRESENTATION_RELATIONSHIP($,$,#11594,#11563)
REPRESENTATION_RELATIONSHIP_WITH_TRANSFORMATION(#43)
SHAPE_REPRESENTATION_RELATIONSHIP()
);
#94=(
REPRESENTATION_RELATIONSHIP($,$,#11595,#11563)
REPRESENTATION_RELATIONSHIP_WITH_TRANSFORMATION(#44)
SHAPE_REPRESENTATION_RELATIONSHIP()
);
#95=(
REPRESENTATION_RELATIONSHIP($,$,#11595,#11563)
REPRESENTATION_RELATIONSHIP_WITH_TRANSFORMATION(#45)
SHAPE_REPRESENTATION_RELATIONSHIP()
);
#96=(
REPRESENTATION_RELATIONSHIP($,$,#11595,#11563)
REPRESENTATION_RELATIONSHIP_WITH_TRANSFORMATION(#46)
SHAPE_REPRESENTATION_RELATIONSHIP()
);
#97=(
REPRESENTATION_RELATIONSHIP($,$,#11595,#11563)
REPRESENTATION_RELATIONSHIP_WITH_TRANSFORMATION(#47)
SHAPE_REPRESENTATION_RELATIONSHIP()
);
#98=(
REPRESENTATION_RELATIONSHIP($,$,#11600,#11563)
REPRESENTATION_RELATIONSHIP_WITH_TRANSFORMATION(#48)
SHAPE_REPRESENTATION_RELATIONSHIP()
);
#99=(
REPRESENTATION_RELATIONSHIP($,$,#11600,#11563)
REPRESENTATION_RELATIONSHIP_WITH_TRANSFORMATION(#49)
SHAPE_REPRESENTATION_RELATIONSHIP()
);
#100=(
REPRESENTATION_RELATIONSHIP($,$,#11600,#11563)
REPRESENTATION_RELATIONSHIP_WITH_TRANSFORMATION(#50)
SHAPE_REPRESENTATION_RELATIONSHIP()
);
#101=(
REPRESENTATION_RELATIONSHIP($,$,#11600,#11563)
REPRESENTATION_RELATIONSHIP_WITH_TRANSFORMATION(#51)
SHAPE_REPRESENTATION_RELATIONSHIP()
);
#102=(
REPRESENTATION_RELATIONSHIP($,$,#11596,#11563)
REPRESENTATION_RELATIONSHIP_WITH_TRANSFORMATION(#52)
SHAPE_REPRESENTATION_RELATIONSHIP()
);
#103=(
REPRESENTATION_RELATIONSHIP($,$,#11596,#11563)
REPRESENTATION_RELATIONSHIP_WITH_TRANSFORMATION(#53)
SHAPE_REPRESENTATION_RELATIONSHIP()
);
#104=(
REPRESENTATION_RELATIONSHIP($,$,#11596,#11563)
REPRESENTATION_RELATIONSHIP_WITH_TRANSFORMATION(#54)
SHAPE_REPRESENTATION_RELATIONSHIP()
);
#105=(
REPRESENTATION_RELATIONSHIP($,$,#11596,#11563)
REPRESENTATION_RELATIONSHIP_WITH_TRANSFORMATION(#55)
SHAPE_REPRESENTATION_RELATIONSHIP()
);
#106=(
REPRESENTATION_RELATIONSHIP($,$,#11599,#11563)
REPRESENTATION_RELATIONSHIP_WITH_TRANSFORMATION(#56)
SHAPE_REPRESENTATION_RELATIONSHIP()
);
#107=(
REPRESENTATION_RELATIONSHIP($,$,#11600,#11563)
REPRESENTATION_RELATIONSHIP_WITH_TRANSFORMATION(#57)
SHAPE_REPRESENTATION_RELATIONSHIP()
);
#108=(
REPRESENTATION_RELATIONSHIP($,$,#11600,#11563)
REPRESENTATION_RELATIONSHIP_WITH_TRANSFORMATION(#58)
SHAPE_REPRESENTATION_RELATIONSHIP()
);
#109=(
REPRESENTATION_RELATIONSHIP($,$,#11600,#11563)
REPRESENTATION_RELATIONSHIP_WITH_TRANSFORMATION(#59)
SHAPE_REPRESENTATION_RELATIONSHIP()
);
#110=(
REPRESENTATION_RELATIONSHIP($,$,#11600,#11563)
REPRESENTATION_RELATIONSHIP_WITH_TRANSFORMATION(#60)
SHAPE_REPRESENTATION_RELATIONSHIP()
);
#111=CONTEXT_DEPENDENT_SHAPE_REPRESENTATION(#61,#11511);
#112=CONTEXT_DEPENDENT_SHAPE_REPRESENTATION(#62,#11512);
#113=CONTEXT_DEPENDENT_SHAPE_REPRESENTATION(#63,#11515);
#114=CONTEXT_DEPENDENT_SHAPE_REPRESENTATION(#64,#11516);
#115=CONTEXT_DEPENDENT_SHAPE_REPRESENTATION(#65,#11517);
#116=CONTEXT_DEPENDENT_SHAPE_REPRESENTATION(#66,#11518);
#117=CONTEXT_DEPENDENT_SHAPE_REPRESENTATION(#67,#11519);
#118=CONTEXT_DEPENDENT_SHAPE_REPRESENTATION(#68,#11520);
#119=CONTEXT_DEPENDENT_SHAPE_REPRESENTATION(#69,#11521);
#120=CONTEXT_DEPENDENT_SHAPE_REPRESENTATION(#70,#11522);
#121=CONTEXT_DEPENDENT_SHAPE_REPRESENTATION(#71,#11523);
#122=CONTEXT_DEPENDENT_SHAPE_REPRESENTATION(#72,#11524);
#123=CONTEXT_DEPENDENT_SHAPE_REPRESENTATION(#73,#11525);
#124=CONTEXT_DEPENDENT_SHAPE_REPRESENTATION(#74,#11526);
#125=CONTEXT_DEPENDENT_SHAPE_REPRESENTATION(#75,#11527);
#126=CONTEXT_DEPENDENT_SHAPE_REPRESENTATION(#76,#11528);
#127=CONTEXT_DEPENDENT_SHAPE_REPRESENTATION(#77,#11529);
#128=CONTEXT_DEPENDENT_SHAPE_REPRESENTATION(#78,#11530);
#129=CONTEXT_DEPENDENT_SHAPE_REPRESENTATION(#79,#11531);
#130=CONTEXT_DEPENDENT_SHAPE_REPRESENTATION(#80,#11532);
#131=CONTEXT_DEPENDENT_SHAPE_REPRESENTATION(#81,#11533);
#132=CONTEXT_DEPENDENT_SHAPE_REPRESENTATION(#82,#11534);
#133=CONTEXT_DEPENDENT_SHAPE_REPRESENTATION(#83,#11535);
#134=CONTEXT_DEPENDENT_SHAPE_REPRESENTATION(#84,#11536);
#135=CONTEXT_DEPENDENT_SHAPE_REPRESENTATION(#85,#11537);
#136=CONTEXT_DEPENDENT_SHAPE_REPRESENTATION(#86,#11538);
#137=CONTEXT_DEPENDENT_SHAPE_REPRESENTATION(#87,#11539);
#138=CONTEXT_DEPENDENT_SHAPE_REPRESENTATION(#88,#11540);
#139=CONTEXT_DEPENDENT_SHAPE_REPRESENTATION(#89,#11541);
#140=CONTEXT_DEPENDENT_SHAPE_REPRESENTATION(#90,#11542);
#141=CONTEXT_DEPENDENT_SHAPE_REPRESENTATION(#91,#11543);
#142=CONTEXT_DEPENDENT_SHAPE_REPRESENTATION(#92,#11544);
#143=CONTEXT_DEPENDENT_SHAPE_REPRESENTATION(#93,#11545);
#144=CONTEXT_DEPENDENT_SHAPE_REPRESENTATION(#94,#11546);
#145=CONTEXT_DEPENDENT_SHAPE_REPRESENTATION(#95,#11547);
#146=CONTEXT_DEPENDENT_SHAPE_REPRESENTATION(#96,#11548);
#147=CONTEXT_DEPENDENT_SHAPE_REPRESENTATION(#97,#11549);
#148=CONTEXT_DEPENDENT_SHAPE_REPRESENTATION(#98,#11550);
#149=CONTEXT_DEPENDENT_SHAPE_REPRESENTATION(#99,#11551);
#150=CONTEXT_DEPENDENT_SHAPE_REPRESENTATION(#100,#11552);
#151=CONTEXT_DEPENDENT_SHAPE_REPRESENTATION(#101,#11553);
#152=CONTEXT_DEPENDENT_SHAPE_REPRESENTATION(#102,#11554);
#153=CONTEXT_DEPENDENT_SHAPE_REPRESENTATION(#103,#11555);
#154=CONTEXT_DEPENDENT_SHAPE_REPRESENTATION(#104,#11556);
#155=CONTEXT_DEPENDENT_SHAPE_REPRESENTATION(#105,#11557);
#156=CONTEXT_DEPENDENT_SHAPE_REPRESENTATION(#106,#11558);
#157=CONTEXT_DEPENDENT_SHAPE_REPRESENTATION(#107,#11559);
#158=CONTEXT_DEPENDENT_SHAPE_REPRESENTATION(#108,#11560);
#159=CONTEXT_DEPENDENT_SHAPE_REPRESENTATION(#109,#11561);
#160=CONTEXT_DEPENDENT_SHAPE_REPRESENTATION(#110,#11562);
#161=NEXT_ASSEMBLY_USAGE_OCCURRENCE('Body:1','Body:1','Body:1',#11635,#11636,
'Body:1');
#162=NEXT_ASSEMBLY_USAGE_OCCURRENCE('Release collar:1',
'Release collar:1','Release collar:1',#11635,#11637,'Release collar:1');
#163=NEXT_ASSEMBLY_USAGE_OCCURRENCE('Base:1','Base:1','Base:1',#11602,#11603,
'Base:1');
#164=NEXT_ASSEMBLY_USAGE_OCCURRENCE('Pedestal:1','Pedestal:1',
'Pedestal:1',#11602,#11604,'Pedestal:1');
#165=NEXT_ASSEMBLY_USAGE_OCCURRENCE('Pedestal (1):1','Pedestal (1):1',
'Pedestal (1):1',#11602,#11605,'Pedestal (1):1');
#166=NEXT_ASSEMBLY_USAGE_OCCURRENCE('Distributor:1','Distributor:1',
'Distributor:1',#11602,#11606,'Distributor:1');
#167=NEXT_ASSEMBLY_USAGE_OCCURRENCE('Outlet tube:1','Outlet tube:1',
'Outlet tube:1',#11602,#11607,'Outlet tube:1');
#168=NEXT_ASSEMBLY_USAGE_OCCURRENCE('Metering plug:1','Metering plug:1',
'Metering plug:1',#11602,#11608,'Metering plug:1');
#169=NEXT_ASSEMBLY_USAGE_OCCURRENCE('Metering stem gasket:1',
'Metering stem gasket:1','Metering stem gasket:1',#11602,#11609,
'Metering stem gasket:1');
#170=NEXT_ASSEMBLY_USAGE_OCCURRENCE('Outlet tube (1):1',
'Outlet tube (1):1','Outlet tube (1):1',#11602,#11610,
'Outlet tube (1):1');
#171=NEXT_ASSEMBLY_USAGE_OCCURRENCE('Metering plug (1):1',
'Metering plug (1):1','Metering plug (1):1',#11602,#11611,
'Metering plug (1):1');
#172=NEXT_ASSEMBLY_USAGE_OCCURRENCE('Metering stem gasket (1):1',
'Metering stem gasket (1):1','Metering stem gasket (1):1',#11602,#11612,
'Metering stem gasket (1):1');
#173=NEXT_ASSEMBLY_USAGE_OCCURRENCE('Outlet tube (2):1',
'Outlet tube (2):1','Outlet tube (2):1',#11602,#11613,
'Outlet tube (2):1');
#174=NEXT_ASSEMBLY_USAGE_OCCURRENCE('Metering plug (2):1',
'Metering plug (2):1','Metering plug (2):1',#11602,#11614,
'Metering plug (2):1');
#175=NEXT_ASSEMBLY_USAGE_OCCURRENCE('Metering stem gasket (2):1',
'Metering stem gasket (2):1','Metering stem gasket (2):1',#11602,#11615,
'Metering stem gasket (2):1');
#176=NEXT_ASSEMBLY_USAGE_OCCURRENCE('Outlet tube (3):1',
'Outlet tube (3):1','Outlet tube (3):1',#11602,#11616,
'Outlet tube (3):1');
#177=NEXT_ASSEMBLY_USAGE_OCCURRENCE('Metering plug (3):1',
'Metering plug (3):1','Metering plug (3):1',#11602,#11617,
'Metering plug (3):1');
#178=NEXT_ASSEMBLY_USAGE_OCCURRENCE('Metering stem gasket (3):1',
'Metering stem gasket (3):1','Metering stem gasket (3):1',#11602,#11618,
'Metering stem gasket (3):1');
#179=NEXT_ASSEMBLY_USAGE_OCCURRENCE('Gallery closure:1',
'Gallery closure:1','Gallery closure:1',#11602,#11619,
'Gallery closure:1');
#180=NEXT_ASSEMBLY_USAGE_OCCURRENCE('Gallery closure (1):1',
'Gallery closure (1):1','Gallery closure (1):1',#11602,#11620,
'Gallery closure (1):1');
#181=NEXT_ASSEMBLY_USAGE_OCCURRENCE('Reservoir:1','Reservoir:1',
'Reservoir:1',#11602,#11621,'Reservoir:1');
#182=NEXT_ASSEMBLY_USAGE_OCCURRENCE('Sight glass gasket:1',
'Sight glass gasket:1','Sight glass gasket:1',#11602,#11622,
'Sight glass gasket:1');
#183=NEXT_ASSEMBLY_USAGE_OCCURRENCE('Sight glass:1','Sight glass:1',
'Sight glass:1',#11602,#11623,'Sight glass:1');
#184=NEXT_ASSEMBLY_USAGE_OCCURRENCE('Sight glass retainer:1',
'Sight glass retainer:1','Sight glass retainer:1',#11602,#11624,
'Sight glass retainer:1');
#185=NEXT_ASSEMBLY_USAGE_OCCURRENCE('M2 sight screw:1',
'M2 sight screw:1','M2 sight screw:1',#11602,#11625,'M2 sight screw:1');
#186=NEXT_ASSEMBLY_USAGE_OCCURRENCE('M2 sight screw (1):1',
'M2 sight screw (1):1','M2 sight screw (1):1',#11602,#11626,
'M2 sight screw (1):1');
#187=NEXT_ASSEMBLY_USAGE_OCCURRENCE('M2 sight screw (2):1',
'M2 sight screw (2):1','M2 sight screw (2):1',#11602,#11627,
'M2 sight screw (2):1');
#188=NEXT_ASSEMBLY_USAGE_OCCURRENCE('M2 sight screw (3):1',
'M2 sight screw (3):1','M2 sight screw (3):1',#11602,#11628,
'M2 sight screw (3):1');
#189=NEXT_ASSEMBLY_USAGE_OCCURRENCE('Lid gasket:1','Lid gasket:1',
'Lid gasket:1',#11602,#11629,'Lid gasket:1');
#190=NEXT_ASSEMBLY_USAGE_OCCURRENCE('Reservoir lid:1','Reservoir lid:1',
'Reservoir lid:1',#11602,#11630,'Reservoir lid:1');
#191=NEXT_ASSEMBLY_USAGE_OCCURRENCE('Vented fill cap:1',
'Vented fill cap:1','Vented fill cap:1',#11602,#11631,
'Vented fill cap:1');
#192=NEXT_ASSEMBLY_USAGE_OCCURRENCE('Bonded foot:1','Bonded foot:1',
'Bonded foot:1',#11602,#11632,'Bonded foot:1');
#193=NEXT_ASSEMBLY_USAGE_OCCURRENCE('Bonded foot (1):1',
'Bonded foot (1):1','Bonded foot (1):1',#11602,#11633,
'Bonded foot (1):1');
#194=NEXT_ASSEMBLY_USAGE_OCCURRENCE('M5x14 Cap Screw:1',
'M5x14 Cap Screw:1','M5x14 Cap Screw:1',#11602,#11634,
'M5x14 Cap Screw:1');
#195=NEXT_ASSEMBLY_USAGE_OCCURRENCE('M5x14 Cap Screw:2',
'M5x14 Cap Screw:2','M5x14 Cap Screw:2',#11602,#11634,
'M5x14 Cap Screw:2');
#196=NEXT_ASSEMBLY_USAGE_OCCURRENCE('M5x14 Cap Screw:3',
'M5x14 Cap Screw:3','M5x14 Cap Screw:3',#11602,#11634,
'M5x14 Cap Screw:3');
#197=NEXT_ASSEMBLY_USAGE_OCCURRENCE('M5x14 Cap Screw:4',
'M5x14 Cap Screw:4','M5x14 Cap Screw:4',#11602,#11634,
'M5x14 Cap Screw:4');
#198=NEXT_ASSEMBLY_USAGE_OCCURRENCE('Cap Screw - M4x16:1',
'Cap Screw - M4x16:1','Cap Screw - M4x16:1',#11602,#11639,
'Cap Screw - M4x16:1');
#199=NEXT_ASSEMBLY_USAGE_OCCURRENCE('Cap Screw - M4x16:2',
'Cap Screw - M4x16:2','Cap Screw - M4x16:2',#11602,#11639,
'Cap Screw - M4x16:2');
#200=NEXT_ASSEMBLY_USAGE_OCCURRENCE('Cap Screw - M4x16:3',
'Cap Screw - M4x16:3','Cap Screw - M4x16:3',#11602,#11639,
'Cap Screw - M4x16:3');
#201=NEXT_ASSEMBLY_USAGE_OCCURRENCE('Cap Screw - M4x16:4',
'Cap Screw - M4x16:4','Cap Screw - M4x16:4',#11602,#11639,
'Cap Screw - M4x16:4');
#202=NEXT_ASSEMBLY_USAGE_OCCURRENCE(
'Push-In Tube Fitting - 6 mm Tube, 1-8 Inch Tapered Pipe Thread:1',
'Push-In Tube Fitting - 6 mm Tube, 1-8 Inch Tapered Pipe Thread:1',
'Push-In Tube Fitting - 6 mm Tube, 1-8 Inch Tapered Pipe Thread:1',#11602,
#11635,
'Push-In Tube Fitting - 6 mm Tube, 1-8 Inch Tapered Pipe Thread:1');
#203=NEXT_ASSEMBLY_USAGE_OCCURRENCE(
'Push-In Tube Fitting - 6 mm Tube, 1-8 Inch Tapered Pipe Thread:2',
'Push-In Tube Fitting - 6 mm Tube, 1-8 Inch Tapered Pipe Thread:2',
'Push-In Tube Fitting - 6 mm Tube, 1-8 Inch Tapered Pipe Thread:2',#11602,
#11635,
'Push-In Tube Fitting - 6 mm Tube, 1-8 Inch Tapered Pipe Thread:2');
#204=NEXT_ASSEMBLY_USAGE_OCCURRENCE(
'Push-In Tube Fitting - 6 mm Tube, 1-8 Inch Tapered Pipe Thread:3',
'Push-In Tube Fitting - 6 mm Tube, 1-8 Inch Tapered Pipe Thread:3',
'Push-In Tube Fitting - 6 mm Tube, 1-8 Inch Tapered Pipe Thread:3',#11602,
#11635,
'Push-In Tube Fitting - 6 mm Tube, 1-8 Inch Tapered Pipe Thread:3');
#205=NEXT_ASSEMBLY_USAGE_OCCURRENCE(
'Push-In Tube Fitting - 6 mm Tube, 1-8 Inch Tapered Pipe Thread:4',
'Push-In Tube Fitting - 6 mm Tube, 1-8 Inch Tapered Pipe Thread:4',
'Push-In Tube Fitting - 6 mm Tube, 1-8 Inch Tapered Pipe Thread:4',#11602,
#11635,
'Push-In Tube Fitting - 6 mm Tube, 1-8 Inch Tapered Pipe Thread:4');
#206=NEXT_ASSEMBLY_USAGE_OCCURRENCE(
'Hex Pipe Nipple - 1-4 Inch Tapered Pipe Thread:1',
'Hex Pipe Nipple - 1-4 Inch Tapered Pipe Thread:1',
'Hex Pipe Nipple - 1-4 Inch Tapered Pipe Thread:1',#11602,#11638,
'Hex Pipe Nipple - 1-4 Inch Tapered Pipe Thread:1');
#207=NEXT_ASSEMBLY_USAGE_OCCURRENCE('Cap Screw - M4x16:5',
'Cap Screw - M4x16:5','Cap Screw - M4x16:5',#11602,#11639,
'Cap Screw - M4x16:5');
#208=NEXT_ASSEMBLY_USAGE_OCCURRENCE('Cap Screw - M4x16:6',
'Cap Screw - M4x16:6','Cap Screw - M4x16:6',#11602,#11639,
'Cap Screw - M4x16:6');
#209=NEXT_ASSEMBLY_USAGE_OCCURRENCE('Cap Screw - M4x16:7',
'Cap Screw - M4x16:7','Cap Screw - M4x16:7',#11602,#11639,
'Cap Screw - M4x16:7');
#210=NEXT_ASSEMBLY_USAGE_OCCURRENCE('Cap Screw - M4x16:8',
'Cap Screw - M4x16:8','Cap Screw - M4x16:8',#11602,#11639,
'Cap Screw - M4x16:8');
#211=CONICAL_SURFACE('',#7106,0.4,0.785398163397448);
#212=CONICAL_SURFACE('',#7110,0.41,0.785398163397448);
#213=CONICAL_SURFACE('',#7114,0.26,0.463647609000806);
#214=CONICAL_SURFACE('',#7177,0.645,0.785398163397448);
#215=CONICAL_SURFACE('',#7180,0.645,0.785398163397448);
#216=CONICAL_SURFACE('',#7188,0.325,0.785398163397448);
#217=CONICAL_SURFACE('',#7192,0.335,0.785398163397448);
#218=CONICAL_SURFACE('',#7196,0.21,0.463647609000806);
#219=CONICAL_SURFACE('',#7200,0.18,0.785398163397448);
#220=ORIENTED_CLOSED_SHELL('',*,#6098,.F.);
#221=ORIENTED_CLOSED_SHELL('',*,#6104,.F.);
#222=BREP_WITH_VOIDS('Body1',#6099,(#220));
#223=BREP_WITH_VOIDS('Body1',#6103,(#221));
#224=B_SPLINE_CURVE_WITH_KNOTS('',3,(#9391,#9392,#9393,#9394,#9395,#9396,
#9397,#9398,#9399,#9400,#9401,#9402),.UNSPECIFIED.,.F.,.F.,(4,2,2,2,2,4),
(-0.95677561507049,-0.896341583425282,-0.835907551780073,-0.715039488489656,
-0.596713648012451,-0.478387807535245),.UNSPECIFIED.);
#225=B_SPLINE_CURVE_WITH_KNOTS('',3,(#9403,#9404,#9405,#9406,#9407,#9408),
 .UNSPECIFIED.,.F.,.F.,(4,2,4),(-1.05899336181655,-1.0172096467157,-0.95677561507049),
 .UNSPECIFIED.);
#226=B_SPLINE_CURVE_WITH_KNOTS('',3,(#9410,#9411,#9412,#9413,#9414,#9415),
 .UNSPECIFIED.,.F.,.F.,(4,2,4),(0.95677561507049,1.0172096467157,1.0589933625076),
 .UNSPECIFIED.);
#227=B_SPLINE_CURVE_WITH_KNOTS('',3,(#9417,#9418,#9419,#9420,#9421,#9422,
#9423,#9424,#9425,#9426,#9427,#9428,#9429,#9430,#9431,#9432,#9433,#9434,
#9435,#9436,#9437,#9438,#9439,#9440,#9441,#9442,#9443),.UNSPECIFIED.,.F.,
 .F.,(4,2,3,2,2,2,2,2,2,2,2,2,4),(-0.102217746746057,-0.0604340316452083,
0.,0.0604340316452084,0.120868063290417,0.241736126580834,0.36006196705804,
0.478387807535245,0.596713648012451,0.715039488489657,0.835907551780073,
0.896341583425282,0.95677561507049),.UNSPECIFIED.);
#228=B_SPLINE_CURVE_WITH_KNOTS('',3,(#9446,#9447,#9448,#9449,#9450,#9451,
#9452,#9453,#9454,#9455,#9456,#9457,#9458,#9459,#9460,#9461,#9462),
 .UNSPECIFIED.,.F.,.F.,(4,2,2,2,2,3,2,4),(-0.478387807535245,-0.360061967058039,
-0.241736126580834,-0.120868063290417,-0.0604340316452083,0.,0.0604340316452084,
0.102217747437108),.UNSPECIFIED.);
#229=B_SPLINE_CURVE_WITH_KNOTS('',3,(#9498,#9499,#9500,#9501,#9502,#9503,
#9504,#9505,#9506,#9507),.UNSPECIFIED.,.F.,.F.,(4,2,2,2,4),(0.,0.0577372801322209,
0.115474560264442,0.173054445763352,0.230634331262262),.UNSPECIFIED.);
#230=B_SPLINE_CURVE_WITH_KNOTS('',3,(#9509,#9510,#9511,#9512,#9513,#9514,
#9515,#9516,#9517,#9518),.UNSPECIFIED.,.F.,.F.,(4,2,2,2,4),(0.691902993786785,
0.749482879285695,0.807062764784605,0.864800044916826,0.922537325049047),
 .UNSPECIFIED.);
#231=B_SPLINE_CURVE_WITH_KNOTS('',3,(#9522,#9523,#9524,#9525,#9526,#9527,
#9528,#9529,#9530,#9531,#9532,#9533,#9534,#9535,#9536,#9537,#9538,#9539),
 .UNSPECIFIED.,.F.,.F.,(4,2,2,2,2,2,2,2,4),(0.230634331262262,0.288214216761172,
0.345794102260082,0.403531382392303,0.461268662524523,0.519005942656744,
0.576743222788965,0.634323108287875,0.691902993786785),.UNSPECIFIED.);
#232=B_SPLINE_CURVE_WITH_KNOTS('',3,(#9553,#9554,#9555,#9556,#9557,#9558,
#9559,#9560,#9561,#9562),.UNSPECIFIED.,.F.,.F.,(4,2,2,2,4),(0.,0.07890547039326,
0.15781094078652,0.235848341776528,0.313885742766535),.UNSPECIFIED.);
#233=B_SPLINE_CURVE_WITH_KNOTS('',3,(#9563,#9564,#9565,#9566,#9567,#9568,
#9569,#9570,#9571,#9572,#9573,#9574,#9575,#9576,#9577,#9578,#9579,#9580,
#9581,#9582,#9583,#9584,#9585,#9586,#9587,#9588),.UNSPECIFIED.,.F.,.F.,
(4,2,2,2,2,2,2,2,2,2,2,2,4),(0.313885742766535,0.391923143756543,0.469960544746551,
0.548866015139811,0.627771485533071,0.706676955926331,0.78558242631959,
0.863619827309598,0.941657228299606,1.01969462928961,1.09773203027962,1.17663750067288,
1.25554297106614),.UNSPECIFIED.);
#234=B_SPLINE_CURVE_WITH_KNOTS('',3,(#9599,#9600,#9601,#9602,#9603,#9604,
#9605,#9606,#9607,#9608),.UNSPECIFIED.,.F.,.F.,(4,2,2,2,4),(0.,0.0577372801322209,
0.115474560264442,0.173054445763352,0.230634331262262),.UNSPECIFIED.);
#235=B_SPLINE_CURVE_WITH_KNOTS('',3,(#9610,#9611,#9612,#9613,#9614,#9615,
#9616,#9617,#9618,#9619),.UNSPECIFIED.,.F.,.F.,(4,2,2,2,4),(0.691902993786785,
0.749482879285695,0.807062764784605,0.864800044916825,0.922537325049046),
 .UNSPECIFIED.);
#236=B_SPLINE_CURVE_WITH_KNOTS('',3,(#9623,#9624,#9625,#9626,#9627,#9628,
#9629,#9630,#9631,#9632,#9633,#9634,#9635,#9636,#9637,#9638,#9639,#9640),
 .UNSPECIFIED.,.F.,.F.,(4,2,2,2,2,2,2,2,4),(0.230634331262262,0.288214216761172,
0.345794102260082,0.403531382392303,0.461268662524523,0.519005942656744,
0.576743222788965,0.634323108287875,0.691902993786785),.UNSPECIFIED.);
#237=B_SPLINE_CURVE_WITH_KNOTS('',3,(#9654,#9655,#9656,#9657,#9658,#9659,
#9660,#9661,#9662,#9663),.UNSPECIFIED.,.F.,.F.,(4,2,2,2,4),(0.,0.0789054703932595,
0.157810940786519,0.235848341776527,0.313885742766535),.UNSPECIFIED.);
#238=B_SPLINE_CURVE_WITH_KNOTS('',3,(#9664,#9665,#9666,#9667,#9668,#9669,
#9670,#9671,#9672,#9673,#9674,#9675,#9676,#9677,#9678,#9679,#9680,#9681,
#9682,#9683,#9684,#9685,#9686,#9687,#9688,#9689),.UNSPECIFIED.,.F.,.F.,
(4,2,2,2,2,2,2,2,2,2,2,2,4),(0.313885742766535,0.391923143756543,0.46996054474655,
0.54886601513981,0.627771485533069,0.706676955926329,0.785582426319588,
0.863619827309596,0.941657228299605,1.01969462928961,1.09773203027962,1.17663750067288,
1.25554297106614),.UNSPECIFIED.);
#239=B_SPLINE_CURVE_WITH_KNOTS('',3,(#9700,#9701,#9702,#9703,#9704,#9705,
#9706,#9707,#9708,#9709),.UNSPECIFIED.,.F.,.F.,(4,2,2,2,4),(0.,0.0577372801322209,
0.115474560264442,0.173054445763352,0.230634331262262),.UNSPECIFIED.);
#240=B_SPLINE_CURVE_WITH_KNOTS('',3,(#9711,#9712,#9713,#9714,#9715,#9716,
#9717,#9718,#9719,#9720),.UNSPECIFIED.,.F.,.F.,(4,2,2,2,4),(0.691902993786785,
0.749482879285695,0.807062764784605,0.864800044916826,0.922537325049047),
 .UNSPECIFIED.);
#241=B_SPLINE_CURVE_WITH_KNOTS('',3,(#9724,#9725,#9726,#9727,#9728,#9729,
#9730,#9731,#9732,#9733,#9734,#9735,#9736,#9737,#9738,#9739,#9740,#9741),
 .UNSPECIFIED.,.F.,.F.,(4,2,2,2,2,2,2,2,4),(0.230634331262262,0.288214216761172,
0.345794102260082,0.403531382392303,0.461268662524523,0.519005942656744,
0.576743222788965,0.634323108287875,0.691902993786785),.UNSPECIFIED.);
#242=B_SPLINE_CURVE_WITH_KNOTS('',3,(#9755,#9756,#9757,#9758,#9759,#9760,
#9761,#9762,#9763,#9764),.UNSPECIFIED.,.F.,.F.,(4,2,2,2,4),(0.,0.0789054703932595,
0.157810940786519,0.235848341776527,0.313885742766535),.UNSPECIFIED.);
#243=B_SPLINE_CURVE_WITH_KNOTS('',3,(#9765,#9766,#9767,#9768,#9769,#9770,
#9771,#9772,#9773,#9774,#9775,#9776,#9777,#9778,#9779,#9780,#9781,#9782,
#9783,#9784,#9785,#9786,#9787,#9788,#9789,#9790),.UNSPECIFIED.,.F.,.F.,
(4,2,2,2,2,2,2,2,2,2,2,2,4),(0.313885742766535,0.391923143756543,0.46996054474655,
0.54886601513981,0.627771485533069,0.706676955926329,0.785582426319588,
0.863619827309596,0.941657228299605,1.01969462928961,1.09773203027962,1.17663750067288,
1.25554297106614),.UNSPECIFIED.);
#244=B_SPLINE_CURVE_WITH_KNOTS('',3,(#9801,#9802,#9803,#9804,#9805,#9806,
#9807,#9808,#9809,#9810),.UNSPECIFIED.,.F.,.F.,(4,2,2,2,4),(0.,0.0577372801322209,
0.115474560264442,0.173054445763352,0.230634331262262),.UNSPECIFIED.);
#245=B_SPLINE_CURVE_WITH_KNOTS('',3,(#9812,#9813,#9814,#9815,#9816,#9817,
#9818,#9819,#9820,#9821),.UNSPECIFIED.,.F.,.F.,(4,2,2,2,4),(0.691902993786786,
0.749482879285696,0.807062764784606,0.864800044916827,0.922537325049048),
 .UNSPECIFIED.);
#246=B_SPLINE_CURVE_WITH_KNOTS('',3,(#9825,#9826,#9827,#9828,#9829,#9830,
#9831,#9832,#9833,#9834,#9835,#9836,#9837,#9838,#9839,#9840,#9841,#9842),
 .UNSPECIFIED.,.F.,.F.,(4,2,2,2,2,2,2,2,4),(0.230634331262262,0.288214216761172,
0.345794102260082,0.403531382392303,0.461268662524524,0.519005942656745,
0.576743222788966,0.634323108287876,0.691902993786786),.UNSPECIFIED.);
#247=B_SPLINE_CURVE_WITH_KNOTS('',3,(#9856,#9857,#9858,#9859,#9860,#9861,
#9862,#9863,#9864,#9865),.UNSPECIFIED.,.F.,.F.,(4,2,2,2,4),(0.,0.07890547039326,
0.15781094078652,0.235848341776528,0.313885742766535),.UNSPECIFIED.);
#248=B_SPLINE_CURVE_WITH_KNOTS('',3,(#9866,#9867,#9868,#9869,#9870,#9871,
#9872,#9873,#9874,#9875,#9876,#9877,#9878,#9879,#9880,#9881,#9882,#9883,
#9884,#9885,#9886,#9887,#9888,#9889,#9890,#9891),.UNSPECIFIED.,.F.,.F.,
(4,2,2,2,2,2,2,2,2,2,2,2,4),(0.313885742766535,0.391923143756543,0.469960544746551,
0.548866015139811,0.627771485533071,0.70667695592633,0.78558242631959,0.863619827309598,
0.941657228299606,1.01969462928961,1.09773203027962,1.17663750067288,1.25554297106614),
 .UNSPECIFIED.);
#249=B_SPLINE_CURVE_WITH_KNOTS('',3,(#10252,#10253,#10254,#10255,#10256,
#10257,#10258,#10259,#10260,#10261,#10262,#10263,#10264,#10265,#10266,#10267,
#10268,#10269,#10270,#10271,#10272,#10273,#10274,#10275,#10276,#10277,#10278,
#10279,#10280,#10281,#10282,#10283,#10284,#10285),.UNSPECIFIED.,.T.,.F.,
(4,2,2,2,2,2,2,2,2,2,2,2,2,2,2,2,4),(0.,0.0300404891334215,0.060080978266843,
0.0918437431465571,0.123606508026271,0.155653989866112,0.187701471705953,
0.217773943328409,0.247846414950866,0.277918886573323,0.30799135819578,
0.34003884003562,0.372086321875461,0.403849086755175,0.435611851634889,
0.465652340768311,0.495692829901732),.UNSPECIFIED.);
#250=B_SPLINE_CURVE_WITH_KNOTS('',3,(#10291,#10292,#10293,#10294,#10295,
#10296,#10297,#10298,#10299,#10300,#10301,#10302,#10303,#10304,#10305,#10306,
#10307,#10308,#10309,#10310,#10311,#10312,#10313,#10314,#10315,#10316,#10317,
#10318,#10319,#10320,#10321,#10322,#10323,#10324),.UNSPECIFIED.,.T.,.F.,
(4,2,2,2,2,2,2,2,2,2,2,2,2,2,2,2,4),(0.,0.0300724716224568,0.0601449432449135,
0.0921924250847542,0.124239906924595,0.156002671804309,0.187765436684023,
0.217805925817445,0.247846414950866,0.277886904084288,0.307927393217709,
0.339690158097423,0.371452922977137,0.403500404816978,0.435547886656819,
0.465620358279276,0.495692829901732),.UNSPECIFIED.);
#251=B_SPLINE_CURVE_WITH_KNOTS('',3,(#10330,#10331,#10332,#10333,#10334,
#10335,#10336,#10337,#10338,#10339,#10340,#10341,#10342,#10343,#10344,#10345,
#10346,#10347,#10348,#10349,#10350,#10351,#10352,#10353,#10354,#10355,#10356,
#10357,#10358,#10359,#10360,#10361,#10362,#10363),.UNSPECIFIED.,.T.,.F.,
(4,2,2,2,2,2,2,2,2,2,2,2,2,2,2,2,4),(0.,0.0300724716224568,0.0601449432449135,
0.0921924250847542,0.124239906924595,0.156002671804309,0.187765436684023,
0.217805925817445,0.247846414950866,0.277886904084288,0.307927393217709,
0.339690158097423,0.371452922977137,0.403500404816978,0.435547886656819,
0.465620358279276,0.495692829901732),.UNSPECIFIED.);
#252=B_SPLINE_CURVE_WITH_KNOTS('',3,(#10369,#10370,#10371,#10372,#10373,
#10374,#10375,#10376,#10377,#10378,#10379,#10380,#10381,#10382,#10383,#10384,
#10385,#10386,#10387,#10388,#10389,#10390,#10391,#10392,#10393,#10394,#10395,
#10396,#10397,#10398,#10399,#10400,#10401,#10402),.UNSPECIFIED.,.T.,.F.,
(4,2,2,2,2,2,2,2,2,2,2,2,2,2,2,2,4),(0.,0.0300404891334215,0.060080978266843,
0.0918437431465571,0.123606508026271,0.155653989866112,0.187701471705953,
0.217773943328409,0.247846414950866,0.277918886573323,0.30799135819578,
0.34003884003562,0.372086321875461,0.403849086755175,0.435611851634889,
0.465652340768311,0.495692829901732),.UNSPECIFIED.);
#253=ELLIPSE('',#6580,0.565685424949238,0.4);
#254=ELLIPSE('',#6581,0.565685424949238,0.4);
#255=ELLIPSE('',#6583,0.565685424949238,0.4);
#256=ELLIPSE('',#6585,0.565685424949238,0.4);
#257=ELLIPSE('',#6586,0.565685424949238,0.4);
#258=ELLIPSE('',#6588,0.565685424949238,0.4);
#259=ELLIPSE('',#6590,0.565685424949238,0.4);
#260=SHAPE_REPRESENTATION_RELATIONSHIP('SRR','None',#11564,#296);
#261=SHAPE_REPRESENTATION_RELATIONSHIP('SRR','None',#11565,#297);
#262=SHAPE_REPRESENTATION_RELATIONSHIP('SRR','None',#11566,#298);
#263=SHAPE_REPRESENTATION_RELATIONSHIP('SRR','None',#11567,#299);
#264=SHAPE_REPRESENTATION_RELATIONSHIP('SRR','None',#11568,#300);
#265=SHAPE_REPRESENTATION_RELATIONSHIP('SRR','None',#11569,#301);
#266=SHAPE_REPRESENTATION_RELATIONSHIP('SRR','None',#11570,#302);
#267=SHAPE_REPRESENTATION_RELATIONSHIP('SRR','None',#11571,#303);
#268=SHAPE_REPRESENTATION_RELATIONSHIP('SRR','None',#11572,#304);
#269=SHAPE_REPRESENTATION_RELATIONSHIP('SRR','None',#11573,#305);
#270=SHAPE_REPRESENTATION_RELATIONSHIP('SRR','None',#11574,#306);
#271=SHAPE_REPRESENTATION_RELATIONSHIP('SRR','None',#11575,#307);
#272=SHAPE_REPRESENTATION_RELATIONSHIP('SRR','None',#11576,#308);
#273=SHAPE_REPRESENTATION_RELATIONSHIP('SRR','None',#11577,#309);
#274=SHAPE_REPRESENTATION_RELATIONSHIP('SRR','None',#11578,#310);
#275=SHAPE_REPRESENTATION_RELATIONSHIP('SRR','None',#11579,#311);
#276=SHAPE_REPRESENTATION_RELATIONSHIP('SRR','None',#11580,#312);
#277=SHAPE_REPRESENTATION_RELATIONSHIP('SRR','None',#11581,#313);
#278=SHAPE_REPRESENTATION_RELATIONSHIP('SRR','None',#11582,#314);
#279=SHAPE_REPRESENTATION_RELATIONSHIP('SRR','None',#11583,#315);
#280=SHAPE_REPRESENTATION_RELATIONSHIP('SRR','None',#11584,#316);
#281=SHAPE_REPRESENTATION_RELATIONSHIP('SRR','None',#11585,#317);
#282=SHAPE_REPRESENTATION_RELATIONSHIP('SRR','None',#11586,#318);
#283=SHAPE_REPRESENTATION_RELATIONSHIP('SRR','None',#11587,#319);
#284=SHAPE_REPRESENTATION_RELATIONSHIP('SRR','None',#11588,#320);
#285=SHAPE_REPRESENTATION_RELATIONSHIP('SRR','None',#11589,#321);
#286=SHAPE_REPRESENTATION_RELATIONSHIP('SRR','None',#11590,#322);
#287=SHAPE_REPRESENTATION_RELATIONSHIP('SRR','None',#11591,#323);
#288=SHAPE_REPRESENTATION_RELATIONSHIP('SRR','None',#11592,#324);
#289=SHAPE_REPRESENTATION_RELATIONSHIP('SRR','None',#11593,#325);
#290=SHAPE_REPRESENTATION_RELATIONSHIP('SRR','None',#11594,#326);
#291=SHAPE_REPRESENTATION_RELATIONSHIP('SRR','None',#11595,#327);
#292=SHAPE_REPRESENTATION_RELATIONSHIP('SRR','None',#11597,#328);
#293=SHAPE_REPRESENTATION_RELATIONSHIP('SRR','None',#11598,#329);
#294=SHAPE_REPRESENTATION_RELATIONSHIP('SRR','None',#11599,#330);
#295=SHAPE_REPRESENTATION_RELATIONSHIP('SRR','None',#11600,#331);
#296=ADVANCED_BREP_SHAPE_REPRESENTATION('',(#368),#11395);
#297=ADVANCED_BREP_SHAPE_REPRESENTATION('',(#369),#11396);
#298=ADVANCED_BREP_SHAPE_REPRESENTATION('',(#370),#11397);
#299=ADVANCED_BREP_SHAPE_REPRESENTATION('',(#371),#11398);
#300=ADVANCED_BREP_SHAPE_REPRESENTATION('',(#372),#11399);
#301=ADVANCED_BREP_SHAPE_REPRESENTATION('',(#373),#11400);
#302=ADVANCED_BREP_SHAPE_REPRESENTATION('',(#374),#11401);
#303=ADVANCED_BREP_SHAPE_REPRESENTATION('',(#375),#11402);
#304=ADVANCED_BREP_SHAPE_REPRESENTATION('',(#376),#11403);
#305=ADVANCED_BREP_SHAPE_REPRESENTATION('',(#377),#11404);
#306=ADVANCED_BREP_SHAPE_REPRESENTATION('',(#378),#11405);
#307=ADVANCED_BREP_SHAPE_REPRESENTATION('',(#379),#11406);
#308=ADVANCED_BREP_SHAPE_REPRESENTATION('',(#380),#11407);
#309=ADVANCED_BREP_SHAPE_REPRESENTATION('',(#381),#11408);
#310=ADVANCED_BREP_SHAPE_REPRESENTATION('',(#382),#11409);
#311=ADVANCED_BREP_SHAPE_REPRESENTATION('',(#383),#11410);
#312=ADVANCED_BREP_SHAPE_REPRESENTATION('',(#384),#11411);
#313=ADVANCED_BREP_SHAPE_REPRESENTATION('',(#385),#11412);
#314=ADVANCED_BREP_SHAPE_REPRESENTATION('',(#386),#11413);
#315=ADVANCED_BREP_SHAPE_REPRESENTATION('',(#387),#11414);
#316=ADVANCED_BREP_SHAPE_REPRESENTATION('',(#388),#11415);
#317=ADVANCED_BREP_SHAPE_REPRESENTATION('',(#389),#11416);
#318=ADVANCED_BREP_SHAPE_REPRESENTATION('',(#390),#11417);
#319=ADVANCED_BREP_SHAPE_REPRESENTATION('',(#391),#11418);
#320=ADVANCED_BREP_SHAPE_REPRESENTATION('',(#392),#11419);
#321=ADVANCED_BREP_SHAPE_REPRESENTATION('',(#393),#11420);
#322=ADVANCED_BREP_SHAPE_REPRESENTATION('',(#394),#11421);
#323=ADVANCED_BREP_SHAPE_REPRESENTATION('',(#395),#11422);
#324=ADVANCED_BREP_SHAPE_REPRESENTATION('',(#396),#11423);
#325=ADVANCED_BREP_SHAPE_REPRESENTATION('',(#397),#11424);
#326=ADVANCED_BREP_SHAPE_REPRESENTATION('',(#398),#11425);
#327=ADVANCED_BREP_SHAPE_REPRESENTATION('',(#222),#11426);
#328=ADVANCED_BREP_SHAPE_REPRESENTATION('',(#399),#11428);
#329=ADVANCED_BREP_SHAPE_REPRESENTATION('',(#400),#11429);
#330=ADVANCED_BREP_SHAPE_REPRESENTATION('',(#401),#11430);
#331=ADVANCED_BREP_SHAPE_REPRESENTATION('',(#223),#11431);
#332=STYLED_ITEM('',(#11798),#368);
#333=STYLED_ITEM('',(#11805),#369);
#334=STYLED_ITEM('',(#11805),#370);
#335=STYLED_ITEM('',(#11833),#371);
#336=STYLED_ITEM('',(#11812),#372);
#337=STYLED_ITEM('',(#11812),#373);
#338=STYLED_ITEM('',(#11833),#374);
#339=STYLED_ITEM('',(#11812),#375);
#340=STYLED_ITEM('',(#11812),#376);
#341=STYLED_ITEM('',(#11833),#377);
#342=STYLED_ITEM('',(#11812),#378);
#343=STYLED_ITEM('',(#11812),#379);
#344=STYLED_ITEM('',(#11833),#380);
#345=STYLED_ITEM('',(#11812),#381);
#346=STYLED_ITEM('',(#11812),#382);
#347=STYLED_ITEM('',(#11833),#383);
#348=STYLED_ITEM('',(#11812),#384);
#349=STYLED_ITEM('',(#11812),#385);
#350=STYLED_ITEM('',(#11812),#386);
#351=STYLED_ITEM('',(#11833),#387);
#352=STYLED_ITEM('',(#11833),#388);
#353=STYLED_ITEM('',(#11812),#389);
#354=STYLED_ITEM('',(#11826),#390);
#355=STYLED_ITEM('',(#11826),#391);
#356=STYLED_ITEM('',(#11826),#392);
#357=STYLED_ITEM('',(#11826),#393);
#358=STYLED_ITEM('',(#11833),#394);
#359=STYLED_ITEM('',(#11805),#395);
#360=STYLED_ITEM('',(#11812),#396);
#361=STYLED_ITEM('',(#11833),#397);
#362=STYLED_ITEM('',(#11833),#398);
#363=STYLED_ITEM('',(#11826),#222);
#364=STYLED_ITEM('',(#11798),#399);
#365=STYLED_ITEM('',(#11833),#400);
#366=STYLED_ITEM('',(#11812),#401);
#367=STYLED_ITEM('',(#11826),#223);
#368=MANIFOLD_SOLID_BREP('Body1',#6067);
#369=MANIFOLD_SOLID_BREP('Body1',#6068);
#370=MANIFOLD_SOLID_BREP('Body1',#6069);
#371=MANIFOLD_SOLID_BREP('Body1',#6070);
#372=MANIFOLD_SOLID_BREP('Body1',#6071);
#373=MANIFOLD_SOLID_BREP('Body1',#6072);
#374=MANIFOLD_SOLID_BREP('Body1',#6073);
#375=MANIFOLD_SOLID_BREP('Body1',#6074);
#376=MANIFOLD_SOLID_BREP('Body1',#6075);
#377=MANIFOLD_SOLID_BREP('Body1',#6076);
#378=MANIFOLD_SOLID_BREP('Body1',#6077);
#379=MANIFOLD_SOLID_BREP('Body1',#6078);
#380=MANIFOLD_SOLID_BREP('Body1',#6079);
#381=MANIFOLD_SOLID_BREP('Body1',#6080);
#382=MANIFOLD_SOLID_BREP('Body1',#6081);
#383=MANIFOLD_SOLID_BREP('Body1',#6082);
#384=MANIFOLD_SOLID_BREP('Body1',#6083);
#385=MANIFOLD_SOLID_BREP('Body1',#6084);
#386=MANIFOLD_SOLID_BREP('Body1',#6085);
#387=MANIFOLD_SOLID_BREP('Body1',#6086);
#388=MANIFOLD_SOLID_BREP('Body1',#6087);
#389=MANIFOLD_SOLID_BREP('Body1',#6088);
#390=MANIFOLD_SOLID_BREP('Body1',#6089);
#391=MANIFOLD_SOLID_BREP('Body1',#6090);
#392=MANIFOLD_SOLID_BREP('Body1',#6091);
#393=MANIFOLD_SOLID_BREP('Body1',#6092);
#394=MANIFOLD_SOLID_BREP('Body1',#6093);
#395=MANIFOLD_SOLID_BREP('Body1',#6094);
#396=MANIFOLD_SOLID_BREP('Body1',#6095);
#397=MANIFOLD_SOLID_BREP('Body1',#6096);
#398=MANIFOLD_SOLID_BREP('Body1',#6097);
#399=MANIFOLD_SOLID_BREP('Body1',#6100);
#400=MANIFOLD_SOLID_BREP('Body1',#6101);
#401=MANIFOLD_SOLID_BREP('Body1',#6102);
#402=FACE_BOUND('',#1177,.T.);
#403=FACE_BOUND('',#1178,.T.);
#404=FACE_BOUND('',#1179,.T.);
#405=FACE_BOUND('',#1180,.T.);
#406=FACE_BOUND('',#1182,.T.);
#407=FACE_BOUND('',#1183,.T.);
#408=FACE_BOUND('',#1184,.T.);
#409=FACE_BOUND('',#1185,.T.);
#410=FACE_BOUND('',#1190,.T.);
#411=FACE_BOUND('',#1193,.T.);
#412=FACE_BOUND('',#1201,.T.);
#413=FACE_BOUND('',#1202,.T.);
#414=FACE_BOUND('',#1203,.T.);
#415=FACE_BOUND('',#1205,.T.);
#416=FACE_BOUND('',#1206,.T.);
#417=FACE_BOUND('',#1211,.T.);
#418=FACE_BOUND('',#1214,.T.);
#419=FACE_BOUND('',#1222,.T.);
#420=FACE_BOUND('',#1223,.T.);
#421=FACE_BOUND('',#1224,.T.);
#422=FACE_BOUND('',#1226,.T.);
#423=FACE_BOUND('',#1227,.T.);
#424=FACE_BOUND('',#1244,.T.);
#425=FACE_BOUND('',#1248,.T.);
#426=FACE_BOUND('',#1252,.T.);
#427=FACE_BOUND('',#1256,.T.);
#428=FACE_BOUND('',#1260,.T.);
#429=FACE_BOUND('',#1264,.T.);
#430=FACE_BOUND('',#1268,.T.);
#431=FACE_BOUND('',#1272,.T.);
#432=FACE_BOUND('',#1276,.T.);
#433=FACE_BOUND('',#1278,.T.);
#434=FACE_BOUND('',#1279,.T.);
#435=FACE_BOUND('',#1280,.T.);
#436=FACE_BOUND('',#1281,.T.);
#437=FACE_BOUND('',#1284,.T.);
#438=FACE_BOUND('',#1287,.T.);
#439=FACE_BOUND('',#1290,.T.);
#440=FACE_BOUND('',#1293,.T.);
#441=FACE_BOUND('',#1300,.T.);
#442=FACE_BOUND('',#1302,.T.);
#443=FACE_BOUND('',#1303,.T.);
#444=FACE_BOUND('',#1304,.T.);
#445=FACE_BOUND('',#1305,.T.);
#446=FACE_BOUND('',#1307,.T.);
#447=FACE_BOUND('',#1309,.T.);
#448=FACE_BOUND('',#1310,.T.);
#449=FACE_BOUND('',#1311,.T.);
#450=FACE_BOUND('',#1312,.T.);
#451=FACE_BOUND('',#1313,.T.);
#452=FACE_BOUND('',#1314,.T.);
#453=FACE_BOUND('',#1315,.T.);
#454=FACE_BOUND('',#1316,.T.);
#455=FACE_BOUND('',#1317,.T.);
#456=FACE_BOUND('',#1319,.T.);
#457=FACE_BOUND('',#1320,.T.);
#458=FACE_BOUND('',#1321,.T.);
#459=FACE_BOUND('',#1322,.T.);
#460=FACE_BOUND('',#1326,.T.);
#461=FACE_BOUND('',#1328,.T.);
#462=FACE_BOUND('',#1330,.T.);
#463=FACE_BOUND('',#1334,.T.);
#464=FACE_BOUND('',#1341,.T.);
#465=FACE_BOUND('',#1343,.T.);
#466=FACE_BOUND('',#1347,.T.);
#467=FACE_BOUND('',#1349,.T.);
#468=FACE_BOUND('',#1351,.T.);
#469=FACE_BOUND('',#1355,.T.);
#470=FACE_BOUND('',#1362,.T.);
#471=FACE_BOUND('',#1364,.T.);
#472=FACE_BOUND('',#1368,.T.);
#473=FACE_BOUND('',#1370,.T.);
#474=FACE_BOUND('',#1372,.T.);
#475=FACE_BOUND('',#1376,.T.);
#476=FACE_BOUND('',#1383,.T.);
#477=FACE_BOUND('',#1385,.T.);
#478=FACE_BOUND('',#1389,.T.);
#479=FACE_BOUND('',#1391,.T.);
#480=FACE_BOUND('',#1393,.T.);
#481=FACE_BOUND('',#1397,.T.);
#482=FACE_BOUND('',#1404,.T.);
#483=FACE_BOUND('',#1406,.T.);
#484=FACE_BOUND('',#1432,.T.);
#485=FACE_BOUND('',#1433,.T.);
#486=FACE_BOUND('',#1439,.T.);
#487=FACE_BOUND('',#1440,.T.);
#488=FACE_BOUND('',#1443,.T.);
#489=FACE_BOUND('',#1444,.T.);
#490=FACE_BOUND('',#1445,.T.);
#491=FACE_BOUND('',#1446,.T.);
#492=FACE_BOUND('',#1448,.T.);
#493=FACE_BOUND('',#1450,.T.);
#494=FACE_BOUND('',#1452,.T.);
#495=FACE_BOUND('',#1453,.T.);
#496=FACE_BOUND('',#1454,.T.);
#497=FACE_BOUND('',#1455,.T.);
#498=FACE_BOUND('',#1456,.T.);
#499=FACE_BOUND('',#1458,.T.);
#500=FACE_BOUND('',#1468,.T.);
#501=FACE_BOUND('',#1469,.T.);
#502=FACE_BOUND('',#1470,.T.);
#503=FACE_BOUND('',#1471,.T.);
#504=FACE_BOUND('',#1472,.T.);
#505=FACE_BOUND('',#1475,.T.);
#506=FACE_BOUND('',#1476,.T.);
#507=FACE_BOUND('',#1477,.T.);
#508=FACE_BOUND('',#1478,.T.);
#509=FACE_BOUND('',#1479,.T.);
#510=FACE_BOUND('',#1488,.T.);
#511=FACE_BOUND('',#1489,.T.);
#512=FACE_BOUND('',#1490,.T.);
#513=FACE_BOUND('',#1491,.T.);
#514=FACE_BOUND('',#1494,.T.);
#515=FACE_BOUND('',#1495,.T.);
#516=FACE_BOUND('',#1496,.T.);
#517=FACE_BOUND('',#1497,.T.);
#518=FACE_BOUND('',#1510,.T.);
#519=FACE_BOUND('',#1511,.T.);
#520=FACE_BOUND('',#1512,.T.);
#521=FACE_BOUND('',#1513,.T.);
#522=FACE_BOUND('',#1514,.T.);
#523=FACE_BOUND('',#1517,.T.);
#524=FACE_BOUND('',#1518,.T.);
#525=FACE_BOUND('',#1519,.T.);
#526=FACE_BOUND('',#1520,.T.);
#527=FACE_BOUND('',#1521,.T.);
#528=FACE_BOUND('',#1531,.T.);
#529=FACE_BOUND('',#1541,.T.);
#530=FACE_BOUND('',#1551,.T.);
#531=FACE_BOUND('',#1561,.T.);
#532=FACE_BOUND('',#1572,.T.);
#533=FACE_BOUND('',#1573,.T.);
#534=FACE_BOUND('',#1574,.T.);
#535=FACE_BOUND('',#1575,.T.);
#536=FACE_BOUND('',#1576,.T.);
#537=FACE_BOUND('',#1578,.T.);
#538=FACE_BOUND('',#1579,.T.);
#539=FACE_BOUND('',#1580,.T.);
#540=FACE_BOUND('',#1581,.T.);
#541=FACE_BOUND('',#1582,.T.);
#542=FACE_BOUND('',#1590,.T.);
#543=FACE_BOUND('',#1591,.T.);
#544=FACE_BOUND('',#1592,.T.);
#545=FACE_BOUND('',#1593,.T.);
#546=FACE_BOUND('',#1594,.T.);
#547=FACE_BOUND('',#1596,.T.);
#548=FACE_BOUND('',#1597,.T.);
#549=FACE_BOUND('',#1598,.T.);
#550=FACE_BOUND('',#1599,.T.);
#551=FACE_BOUND('',#1600,.T.);
#552=FACE_BOUND('',#1603,.T.);
#553=FACE_BOUND('',#1606,.T.);
#554=FACE_BOUND('',#1609,.T.);
#555=FACE_BOUND('',#1636,.T.);
#556=FACE_BOUND('',#1641,.T.);
#557=FACE_BOUND('',#1643,.T.);
#558=FACE_BOUND('',#1645,.T.);
#559=FACE_BOUND('',#1653,.T.);
#560=FACE_BOUND('',#1656,.T.);
#561=FACE_BOUND('',#1660,.T.);
#562=FACE_BOUND('',#1663,.T.);
#563=FACE_BOUND('',#1666,.T.);
#564=FACE_BOUND('',#1669,.T.);
#565=FACE_BOUND('',#1672,.T.);
#566=FACE_BOUND('',#1674,.T.);
#567=FACE_BOUND('',#1683,.T.);
#568=FACE_BOUND('',#1688,.T.);
#569=FACE_BOUND('',#1695,.T.);
#570=PLANE('',#6516);
#571=PLANE('',#6517);
#572=PLANE('',#6518);
#573=PLANE('',#6519);
#574=PLANE('',#6520);
#575=PLANE('',#6521);
#576=PLANE('',#6526);
#577=PLANE('',#6530);
#578=PLANE('',#6535);
#579=PLANE('',#6541);
#580=PLANE('',#6542);
#581=PLANE('',#6543);
#582=PLANE('',#6544);
#583=PLANE('',#6545);
#584=PLANE('',#6546);
#585=PLANE('',#6551);
#586=PLANE('',#6555);
#587=PLANE('',#6560);
#588=PLANE('',#6566);
#589=PLANE('',#6567);
#590=PLANE('',#6568);
#591=PLANE('',#6569);
#592=PLANE('',#6570);
#593=PLANE('',#6571);
#594=PLANE('',#6573);
#595=PLANE('',#6575);
#596=PLANE('',#6577);
#597=PLANE('',#6591);
#598=PLANE('',#6592);
#599=PLANE('',#6593);
#600=PLANE('',#6595);
#601=PLANE('',#6602);
#602=PLANE('',#6606);
#603=PLANE('',#6612);
#604=PLANE('',#6618);
#605=PLANE('',#6624);
#606=PLANE('',#6630);
#607=PLANE('',#6636);
#608=PLANE('',#6642);
#609=PLANE('',#6648);
#610=PLANE('',#6654);
#611=PLANE('',#6661);
#612=PLANE('',#6666);
#613=PLANE('',#6671);
#614=PLANE('',#6676);
#615=PLANE('',#6686);
#616=PLANE('',#6687);
#617=PLANE('',#6688);
#618=PLANE('',#6689);
#619=PLANE('',#6690);
#620=PLANE('',#6691);
#621=PLANE('',#6699);
#622=PLANE('',#6700);
#623=PLANE('',#6702);
#624=PLANE('',#6707);
#625=PLANE('',#6708);
#626=PLANE('',#6714);
#627=PLANE('',#6722);
#628=PLANE('',#6723);
#629=PLANE('',#6731);
#630=PLANE('',#6732);
#631=PLANE('',#6734);
#632=PLANE('',#6739);
#633=PLANE('',#6740);
#634=PLANE('',#6746);
#635=PLANE('',#6754);
#636=PLANE('',#6755);
#637=PLANE('',#6763);
#638=PLANE('',#6764);
#639=PLANE('',#6766);
#640=PLANE('',#6771);
#641=PLANE('',#6772);
#642=PLANE('',#6778);
#643=PLANE('',#6786);
#644=PLANE('',#6787);
#645=PLANE('',#6795);
#646=PLANE('',#6796);
#647=PLANE('',#6798);
#648=PLANE('',#6803);
#649=PLANE('',#6804);
#650=PLANE('',#6810);
#651=PLANE('',#6818);
#652=PLANE('',#6819);
#653=PLANE('',#6824);
#654=PLANE('',#6825);
#655=PLANE('',#6830);
#656=PLANE('',#6831);
#657=PLANE('',#6836);
#658=PLANE('',#6840);
#659=PLANE('',#6844);
#660=PLANE('',#6848);
#661=PLANE('',#6857);
#662=PLANE('',#6858);
#663=PLANE('',#6860);
#664=PLANE('',#6862);
#665=PLANE('',#6864);
#666=PLANE('',#6865);
#667=PLANE('',#6867);
#668=PLANE('',#6868);
#669=PLANE('',#6869);
#670=PLANE('',#6871);
#671=PLANE('',#6872);
#672=PLANE('',#6874);
#673=PLANE('',#6881);
#674=PLANE('',#6885);
#675=PLANE('',#6886);
#676=PLANE('',#6900);
#677=PLANE('',#6901);
#678=PLANE('',#6902);
#679=PLANE('',#6903);
#680=PLANE('',#6904);
#681=PLANE('',#6905);
#682=PLANE('',#6906);
#683=PLANE('',#6907);
#684=PLANE('',#6908);
#685=PLANE('',#6909);
#686=PLANE('',#6923);
#687=PLANE('',#6924);
#688=PLANE('',#6925);
#689=PLANE('',#6926);
#690=PLANE('',#6927);
#691=PLANE('',#6928);
#692=PLANE('',#6942);
#693=PLANE('',#6943);
#694=PLANE('',#6944);
#695=PLANE('',#6945);
#696=PLANE('',#6946);
#697=PLANE('',#6947);
#698=PLANE('',#6948);
#699=PLANE('',#6949);
#700=PLANE('',#6950);
#701=PLANE('',#6951);
#702=PLANE('',#6953);
#703=PLANE('',#6954);
#704=PLANE('',#6955);
#705=PLANE('',#6958);
#706=PLANE('',#6960);
#707=PLANE('',#6963);
#708=PLANE('',#6969);
#709=PLANE('',#6971);
#710=PLANE('',#6972);
#711=PLANE('',#6973);
#712=PLANE('',#6976);
#713=PLANE('',#6978);
#714=PLANE('',#6981);
#715=PLANE('',#6987);
#716=PLANE('',#6989);
#717=PLANE('',#6990);
#718=PLANE('',#6991);
#719=PLANE('',#6994);
#720=PLANE('',#6996);
#721=PLANE('',#6999);
#722=PLANE('',#7005);
#723=PLANE('',#7007);
#724=PLANE('',#7008);
#725=PLANE('',#7009);
#726=PLANE('',#7012);
#727=PLANE('',#7014);
#728=PLANE('',#7017);
#729=PLANE('',#7023);
#730=PLANE('',#7043);
#731=PLANE('',#7044);
#732=PLANE('',#7064);
#733=PLANE('',#7065);
#734=PLANE('',#7070);
#735=PLANE('',#7075);
#736=PLANE('',#7078);
#737=PLANE('',#7080);
#738=PLANE('',#7081);
#739=PLANE('',#7082);
#740=PLANE('',#7083);
#741=PLANE('',#7084);
#742=PLANE('',#7085);
#743=PLANE('',#7087);
#744=PLANE('',#7088);
#745=PLANE('',#7089);
#746=PLANE('',#7090);
#747=PLANE('',#7091);
#748=PLANE('',#7092);
#749=PLANE('',#7094);
#750=PLANE('',#7095);
#751=PLANE('',#7096);
#752=PLANE('',#7097);
#753=PLANE('',#7098);
#754=PLANE('',#7099);
#755=PLANE('',#7100);
#756=PLANE('',#7101);
#757=PLANE('',#7102);
#758=PLANE('',#7104);
#759=PLANE('',#7112);
#760=PLANE('',#7122);
#761=PLANE('',#7124);
#762=PLANE('',#7126);
#763=PLANE('',#7128);
#764=PLANE('',#7129);
#765=PLANE('',#7130);
#766=PLANE('',#7131);
#767=PLANE('',#7132);
#768=PLANE('',#7133);
#769=PLANE('',#7134);
#770=PLANE('',#7138);
#771=PLANE('',#7143);
#772=PLANE('',#7147);
#773=PLANE('',#7152);
#774=PLANE('',#7156);
#775=PLANE('',#7162);
#776=PLANE('',#7164);
#777=PLANE('',#7166);
#778=PLANE('',#7167);
#779=PLANE('',#7168);
#780=PLANE('',#7169);
#781=PLANE('',#7170);
#782=PLANE('',#7171);
#783=PLANE('',#7174);
#784=PLANE('',#7182);
#785=PLANE('',#7186);
#786=PLANE('',#7194);
#787=PLANE('',#7202);
#788=PLANE('',#7203);
#789=PLANE('',#7204);
#790=PLANE('',#7205);
#791=PLANE('',#7206);
#792=PLANE('',#7207);
#793=PLANE('',#7208);
#794=PLANE('',#7209);
#795=PLANE('',#7210);
#796=FACE_OUTER_BOUND('',#1168,.T.);
#797=FACE_OUTER_BOUND('',#1169,.T.);
#798=FACE_OUTER_BOUND('',#1170,.T.);
#799=FACE_OUTER_BOUND('',#1171,.T.);
#800=FACE_OUTER_BOUND('',#1172,.T.);
#801=FACE_OUTER_BOUND('',#1173,.T.);
#802=FACE_OUTER_BOUND('',#1174,.T.);
#803=FACE_OUTER_BOUND('',#1175,.T.);
#804=FACE_OUTER_BOUND('',#1176,.T.);
#805=FACE_OUTER_BOUND('',#1181,.T.);
#806=FACE_OUTER_BOUND('',#1186,.T.);
#807=FACE_OUTER_BOUND('',#1187,.T.);
#808=FACE_OUTER_BOUND('',#1188,.T.);
#809=FACE_OUTER_BOUND('',#1189,.T.);
#810=FACE_OUTER_BOUND('',#1191,.T.);
#811=FACE_OUTER_BOUND('',#1192,.T.);
#812=FACE_OUTER_BOUND('',#1194,.T.);
#813=FACE_OUTER_BOUND('',#1195,.T.);
#814=FACE_OUTER_BOUND('',#1196,.T.);
#815=FACE_OUTER_BOUND('',#1197,.T.);
#816=FACE_OUTER_BOUND('',#1198,.T.);
#817=FACE_OUTER_BOUND('',#1199,.T.);
#818=FACE_OUTER_BOUND('',#1200,.T.);
#819=FACE_OUTER_BOUND('',#1204,.T.);
#820=FACE_OUTER_BOUND('',#1207,.T.);
#821=FACE_OUTER_BOUND('',#1208,.T.);
#822=FACE_OUTER_BOUND('',#1209,.T.);
#823=FACE_OUTER_BOUND('',#1210,.T.);
#824=FACE_OUTER_BOUND('',#1212,.T.);
#825=FACE_OUTER_BOUND('',#1213,.T.);
#826=FACE_OUTER_BOUND('',#1215,.T.);
#827=FACE_OUTER_BOUND('',#1216,.T.);
#828=FACE_OUTER_BOUND('',#1217,.T.);
#829=FACE_OUTER_BOUND('',#1218,.T.);
#830=FACE_OUTER_BOUND('',#1219,.T.);
#831=FACE_OUTER_BOUND('',#1220,.T.);
#832=FACE_OUTER_BOUND('',#1221,.T.);
#833=FACE_OUTER_BOUND('',#1225,.T.);
#834=FACE_OUTER_BOUND('',#1228,.T.);
#835=FACE_OUTER_BOUND('',#1229,.T.);
#836=FACE_OUTER_BOUND('',#1230,.T.);
#837=FACE_OUTER_BOUND('',#1231,.T.);
#838=FACE_OUTER_BOUND('',#1232,.T.);
#839=FACE_OUTER_BOUND('',#1233,.T.);
#840=FACE_OUTER_BOUND('',#1234,.T.);
#841=FACE_OUTER_BOUND('',#1235,.T.);
#842=FACE_OUTER_BOUND('',#1236,.T.);
#843=FACE_OUTER_BOUND('',#1237,.T.);
#844=FACE_OUTER_BOUND('',#1238,.T.);
#845=FACE_OUTER_BOUND('',#1239,.T.);
#846=FACE_OUTER_BOUND('',#1240,.T.);
#847=FACE_OUTER_BOUND('',#1241,.T.);
#848=FACE_OUTER_BOUND('',#1242,.T.);
#849=FACE_OUTER_BOUND('',#1243,.T.);
#850=FACE_OUTER_BOUND('',#1245,.T.);
#851=FACE_OUTER_BOUND('',#1246,.T.);
#852=FACE_OUTER_BOUND('',#1247,.T.);
#853=FACE_OUTER_BOUND('',#1249,.T.);
#854=FACE_OUTER_BOUND('',#1250,.T.);
#855=FACE_OUTER_BOUND('',#1251,.T.);
#856=FACE_OUTER_BOUND('',#1253,.T.);
#857=FACE_OUTER_BOUND('',#1254,.T.);
#858=FACE_OUTER_BOUND('',#1255,.T.);
#859=FACE_OUTER_BOUND('',#1257,.T.);
#860=FACE_OUTER_BOUND('',#1258,.T.);
#861=FACE_OUTER_BOUND('',#1259,.T.);
#862=FACE_OUTER_BOUND('',#1261,.T.);
#863=FACE_OUTER_BOUND('',#1262,.T.);
#864=FACE_OUTER_BOUND('',#1263,.T.);
#865=FACE_OUTER_BOUND('',#1265,.T.);
#866=FACE_OUTER_BOUND('',#1266,.T.);
#867=FACE_OUTER_BOUND('',#1267,.T.);
#868=FACE_OUTER_BOUND('',#1269,.T.);
#869=FACE_OUTER_BOUND('',#1270,.T.);
#870=FACE_OUTER_BOUND('',#1271,.T.);
#871=FACE_OUTER_BOUND('',#1273,.T.);
#872=FACE_OUTER_BOUND('',#1274,.T.);
#873=FACE_OUTER_BOUND('',#1275,.T.);
#874=FACE_OUTER_BOUND('',#1277,.T.);
#875=FACE_OUTER_BOUND('',#1282,.T.);
#876=FACE_OUTER_BOUND('',#1283,.T.);
#877=FACE_OUTER_BOUND('',#1285,.T.);
#878=FACE_OUTER_BOUND('',#1286,.T.);
#879=FACE_OUTER_BOUND('',#1288,.T.);
#880=FACE_OUTER_BOUND('',#1289,.T.);
#881=FACE_OUTER_BOUND('',#1291,.T.);
#882=FACE_OUTER_BOUND('',#1292,.T.);
#883=FACE_OUTER_BOUND('',#1294,.T.);
#884=FACE_OUTER_BOUND('',#1295,.T.);
#885=FACE_OUTER_BOUND('',#1296,.T.);
#886=FACE_OUTER_BOUND('',#1297,.T.);
#887=FACE_OUTER_BOUND('',#1298,.T.);
#888=FACE_OUTER_BOUND('',#1299,.T.);
#889=FACE_OUTER_BOUND('',#1301,.T.);
#890=FACE_OUTER_BOUND('',#1306,.T.);
#891=FACE_OUTER_BOUND('',#1308,.T.);
#892=FACE_OUTER_BOUND('',#1318,.T.);
#893=FACE_OUTER_BOUND('',#1323,.T.);
#894=FACE_OUTER_BOUND('',#1324,.T.);
#895=FACE_OUTER_BOUND('',#1325,.T.);
#896=FACE_OUTER_BOUND('',#1327,.T.);
#897=FACE_OUTER_BOUND('',#1329,.T.);
#898=FACE_OUTER_BOUND('',#1331,.T.);
#899=FACE_OUTER_BOUND('',#1332,.T.);
#900=FACE_OUTER_BOUND('',#1333,.T.);
#901=FACE_OUTER_BOUND('',#1335,.T.);
#902=FACE_OUTER_BOUND('',#1336,.T.);
#903=FACE_OUTER_BOUND('',#1337,.T.);
#904=FACE_OUTER_BOUND('',#1338,.T.);
#905=FACE_OUTER_BOUND('',#1339,.T.);
#906=FACE_OUTER_BOUND('',#1340,.T.);
#907=FACE_OUTER_BOUND('',#1342,.T.);
#908=FACE_OUTER_BOUND('',#1344,.T.);
#909=FACE_OUTER_BOUND('',#1345,.T.);
#910=FACE_OUTER_BOUND('',#1346,.T.);
#911=FACE_OUTER_BOUND('',#1348,.T.);
#912=FACE_OUTER_BOUND('',#1350,.T.);
#913=FACE_OUTER_BOUND('',#1352,.T.);
#914=FACE_OUTER_BOUND('',#1353,.T.);
#915=FACE_OUTER_BOUND('',#1354,.T.);
#916=FACE_OUTER_BOUND('',#1356,.T.);
#917=FACE_OUTER_BOUND('',#1357,.T.);
#918=FACE_OUTER_BOUND('',#1358,.T.);
#919=FACE_OUTER_BOUND('',#1359,.T.);
#920=FACE_OUTER_BOUND('',#1360,.T.);
#921=FACE_OUTER_BOUND('',#1361,.T.);
#922=FACE_OUTER_BOUND('',#1363,.T.);
#923=FACE_OUTER_BOUND('',#1365,.T.);
#924=FACE_OUTER_BOUND('',#1366,.T.);
#925=FACE_OUTER_BOUND('',#1367,.T.);
#926=FACE_OUTER_BOUND('',#1369,.T.);
#927=FACE_OUTER_BOUND('',#1371,.T.);
#928=FACE_OUTER_BOUND('',#1373,.T.);
#929=FACE_OUTER_BOUND('',#1374,.T.);
#930=FACE_OUTER_BOUND('',#1375,.T.);
#931=FACE_OUTER_BOUND('',#1377,.T.);
#932=FACE_OUTER_BOUND('',#1378,.T.);
#933=FACE_OUTER_BOUND('',#1379,.T.);
#934=FACE_OUTER_BOUND('',#1380,.T.);
#935=FACE_OUTER_BOUND('',#1381,.T.);
#936=FACE_OUTER_BOUND('',#1382,.T.);
#937=FACE_OUTER_BOUND('',#1384,.T.);
#938=FACE_OUTER_BOUND('',#1386,.T.);
#939=FACE_OUTER_BOUND('',#1387,.T.);
#940=FACE_OUTER_BOUND('',#1388,.T.);
#941=FACE_OUTER_BOUND('',#1390,.T.);
#942=FACE_OUTER_BOUND('',#1392,.T.);
#943=FACE_OUTER_BOUND('',#1394,.T.);
#944=FACE_OUTER_BOUND('',#1395,.T.);
#945=FACE_OUTER_BOUND('',#1396,.T.);
#946=FACE_OUTER_BOUND('',#1398,.T.);
#947=FACE_OUTER_BOUND('',#1399,.T.);
#948=FACE_OUTER_BOUND('',#1400,.T.);
#949=FACE_OUTER_BOUND('',#1401,.T.);
#950=FACE_OUTER_BOUND('',#1402,.T.);
#951=FACE_OUTER_BOUND('',#1403,.T.);
#952=FACE_OUTER_BOUND('',#1405,.T.);
#953=FACE_OUTER_BOUND('',#1407,.T.);
#954=FACE_OUTER_BOUND('',#1408,.T.);
#955=FACE_OUTER_BOUND('',#1409,.T.);
#956=FACE_OUTER_BOUND('',#1410,.T.);
#957=FACE_OUTER_BOUND('',#1411,.T.);
#958=FACE_OUTER_BOUND('',#1412,.T.);
#959=FACE_OUTER_BOUND('',#1413,.T.);
#960=FACE_OUTER_BOUND('',#1414,.T.);
#961=FACE_OUTER_BOUND('',#1415,.T.);
#962=FACE_OUTER_BOUND('',#1416,.T.);
#963=FACE_OUTER_BOUND('',#1417,.T.);
#964=FACE_OUTER_BOUND('',#1418,.T.);
#965=FACE_OUTER_BOUND('',#1419,.T.);
#966=FACE_OUTER_BOUND('',#1420,.T.);
#967=FACE_OUTER_BOUND('',#1421,.T.);
#968=FACE_OUTER_BOUND('',#1422,.T.);
#969=FACE_OUTER_BOUND('',#1423,.T.);
#970=FACE_OUTER_BOUND('',#1424,.T.);
#971=FACE_OUTER_BOUND('',#1425,.T.);
#972=FACE_OUTER_BOUND('',#1426,.T.);
#973=FACE_OUTER_BOUND('',#1427,.T.);
#974=FACE_OUTER_BOUND('',#1428,.T.);
#975=FACE_OUTER_BOUND('',#1429,.T.);
#976=FACE_OUTER_BOUND('',#1430,.T.);
#977=FACE_OUTER_BOUND('',#1431,.T.);
#978=FACE_OUTER_BOUND('',#1434,.T.);
#979=FACE_OUTER_BOUND('',#1435,.T.);
#980=FACE_OUTER_BOUND('',#1436,.T.);
#981=FACE_OUTER_BOUND('',#1437,.T.);
#982=FACE_OUTER_BOUND('',#1438,.T.);
#983=FACE_OUTER_BOUND('',#1441,.T.);
#984=FACE_OUTER_BOUND('',#1442,.T.);
#985=FACE_OUTER_BOUND('',#1447,.T.);
#986=FACE_OUTER_BOUND('',#1449,.T.);
#987=FACE_OUTER_BOUND('',#1451,.T.);
#988=FACE_OUTER_BOUND('',#1457,.T.);
#989=FACE_OUTER_BOUND('',#1459,.T.);
#990=FACE_OUTER_BOUND('',#1460,.T.);
#991=FACE_OUTER_BOUND('',#1461,.T.);
#992=FACE_OUTER_BOUND('',#1462,.T.);
#993=FACE_OUTER_BOUND('',#1463,.T.);
#994=FACE_OUTER_BOUND('',#1464,.T.);
#995=FACE_OUTER_BOUND('',#1465,.T.);
#996=FACE_OUTER_BOUND('',#1466,.T.);
#997=FACE_OUTER_BOUND('',#1467,.T.);
#998=FACE_OUTER_BOUND('',#1473,.T.);
#999=FACE_OUTER_BOUND('',#1474,.T.);
#1000=FACE_OUTER_BOUND('',#1480,.T.);
#1001=FACE_OUTER_BOUND('',#1481,.T.);
#1002=FACE_OUTER_BOUND('',#1482,.T.);
#1003=FACE_OUTER_BOUND('',#1483,.T.);
#1004=FACE_OUTER_BOUND('',#1484,.T.);
#1005=FACE_OUTER_BOUND('',#1485,.T.);
#1006=FACE_OUTER_BOUND('',#1486,.T.);
#1007=FACE_OUTER_BOUND('',#1487,.T.);
#1008=FACE_OUTER_BOUND('',#1492,.T.);
#1009=FACE_OUTER_BOUND('',#1493,.T.);
#1010=FACE_OUTER_BOUND('',#1498,.T.);
#1011=FACE_OUTER_BOUND('',#1499,.T.);
#1012=FACE_OUTER_BOUND('',#1500,.T.);
#1013=FACE_OUTER_BOUND('',#1501,.T.);
#1014=FACE_OUTER_BOUND('',#1502,.T.);
#1015=FACE_OUTER_BOUND('',#1503,.T.);
#1016=FACE_OUTER_BOUND('',#1504,.T.);
#1017=FACE_OUTER_BOUND('',#1505,.T.);
#1018=FACE_OUTER_BOUND('',#1506,.T.);
#1019=FACE_OUTER_BOUND('',#1507,.T.);
#1020=FACE_OUTER_BOUND('',#1508,.T.);
#1021=FACE_OUTER_BOUND('',#1509,.T.);
#1022=FACE_OUTER_BOUND('',#1515,.T.);
#1023=FACE_OUTER_BOUND('',#1516,.T.);
#1024=FACE_OUTER_BOUND('',#1522,.T.);
#1025=FACE_OUTER_BOUND('',#1523,.T.);
#1026=FACE_OUTER_BOUND('',#1524,.T.);
#1027=FACE_OUTER_BOUND('',#1525,.T.);
#1028=FACE_OUTER_BOUND('',#1526,.T.);
#1029=FACE_OUTER_BOUND('',#1527,.T.);
#1030=FACE_OUTER_BOUND('',#1528,.T.);
#1031=FACE_OUTER_BOUND('',#1529,.T.);
#1032=FACE_OUTER_BOUND('',#1530,.T.);
#1033=FACE_OUTER_BOUND('',#1532,.T.);
#1034=FACE_OUTER_BOUND('',#1533,.T.);
#1035=FACE_OUTER_BOUND('',#1534,.T.);
#1036=FACE_OUTER_BOUND('',#1535,.T.);
#1037=FACE_OUTER_BOUND('',#1536,.T.);
#1038=FACE_OUTER_BOUND('',#1537,.T.);
#1039=FACE_OUTER_BOUND('',#1538,.T.);
#1040=FACE_OUTER_BOUND('',#1539,.T.);
#1041=FACE_OUTER_BOUND('',#1540,.T.);
#1042=FACE_OUTER_BOUND('',#1542,.T.);
#1043=FACE_OUTER_BOUND('',#1543,.T.);
#1044=FACE_OUTER_BOUND('',#1544,.T.);
#1045=FACE_OUTER_BOUND('',#1545,.T.);
#1046=FACE_OUTER_BOUND('',#1546,.T.);
#1047=FACE_OUTER_BOUND('',#1547,.T.);
#1048=FACE_OUTER_BOUND('',#1548,.T.);
#1049=FACE_OUTER_BOUND('',#1549,.T.);
#1050=FACE_OUTER_BOUND('',#1550,.T.);
#1051=FACE_OUTER_BOUND('',#1552,.T.);
#1052=FACE_OUTER_BOUND('',#1553,.T.);
#1053=FACE_OUTER_BOUND('',#1554,.T.);
#1054=FACE_OUTER_BOUND('',#1555,.T.);
#1055=FACE_OUTER_BOUND('',#1556,.T.);
#1056=FACE_OUTER_BOUND('',#1557,.T.);
#1057=FACE_OUTER_BOUND('',#1558,.T.);
#1058=FACE_OUTER_BOUND('',#1559,.T.);
#1059=FACE_OUTER_BOUND('',#1560,.T.);
#1060=FACE_OUTER_BOUND('',#1562,.T.);
#1061=FACE_OUTER_BOUND('',#1563,.T.);
#1062=FACE_OUTER_BOUND('',#1564,.T.);
#1063=FACE_OUTER_BOUND('',#1565,.T.);
#1064=FACE_OUTER_BOUND('',#1566,.T.);
#1065=FACE_OUTER_BOUND('',#1567,.T.);
#1066=FACE_OUTER_BOUND('',#1568,.T.);
#1067=FACE_OUTER_BOUND('',#1569,.T.);
#1068=FACE_OUTER_BOUND('',#1570,.T.);
#1069=FACE_OUTER_BOUND('',#1571,.T.);
#1070=FACE_OUTER_BOUND('',#1577,.T.);
#1071=FACE_OUTER_BOUND('',#1583,.T.);
#1072=FACE_OUTER_BOUND('',#1584,.T.);
#1073=FACE_OUTER_BOUND('',#1585,.T.);
#1074=FACE_OUTER_BOUND('',#1586,.T.);
#1075=FACE_OUTER_BOUND('',#1587,.T.);
#1076=FACE_OUTER_BOUND('',#1588,.T.);
#1077=FACE_OUTER_BOUND('',#1589,.T.);
#1078=FACE_OUTER_BOUND('',#1595,.T.);
#1079=FACE_OUTER_BOUND('',#1601,.T.);
#1080=FACE_OUTER_BOUND('',#1602,.T.);
#1081=FACE_OUTER_BOUND('',#1604,.T.);
#1082=FACE_OUTER_BOUND('',#1605,.T.);
#1083=FACE_OUTER_BOUND('',#1607,.T.);
#1084=FACE_OUTER_BOUND('',#1608,.T.);
#1085=FACE_OUTER_BOUND('',#1610,.T.);
#1086=FACE_OUTER_BOUND('',#1611,.T.);
#1087=FACE_OUTER_BOUND('',#1612,.T.);
#1088=FACE_OUTER_BOUND('',#1613,.T.);
#1089=FACE_OUTER_BOUND('',#1614,.T.);
#1090=FACE_OUTER_BOUND('',#1615,.T.);
#1091=FACE_OUTER_BOUND('',#1616,.T.);
#1092=FACE_OUTER_BOUND('',#1617,.T.);
#1093=FACE_OUTER_BOUND('',#1618,.T.);
#1094=FACE_OUTER_BOUND('',#1619,.T.);
#1095=FACE_OUTER_BOUND('',#1620,.T.);
#1096=FACE_OUTER_BOUND('',#1621,.T.);
#1097=FACE_OUTER_BOUND('',#1622,.T.);
#1098=FACE_OUTER_BOUND('',#1623,.T.);
#1099=FACE_OUTER_BOUND('',#1624,.T.);
#1100=FACE_OUTER_BOUND('',#1625,.T.);
#1101=FACE_OUTER_BOUND('',#1626,.T.);
#1102=FACE_OUTER_BOUND('',#1627,.T.);
#1103=FACE_OUTER_BOUND('',#1628,.T.);
#1104=FACE_OUTER_BOUND('',#1629,.T.);
#1105=FACE_OUTER_BOUND('',#1630,.T.);
#1106=FACE_OUTER_BOUND('',#1631,.T.);
#1107=FACE_OUTER_BOUND('',#1632,.T.);
#1108=FACE_OUTER_BOUND('',#1633,.T.);
#1109=FACE_OUTER_BOUND('',#1634,.T.);
#1110=FACE_OUTER_BOUND('',#1635,.T.);
#1111=FACE_OUTER_BOUND('',#1637,.T.);
#1112=FACE_OUTER_BOUND('',#1638,.T.);
#1113=FACE_OUTER_BOUND('',#1639,.T.);
#1114=FACE_OUTER_BOUND('',#1640,.T.);
#1115=FACE_OUTER_BOUND('',#1642,.T.);
#1116=FACE_OUTER_BOUND('',#1644,.T.);
#1117=FACE_OUTER_BOUND('',#1646,.T.);
#1118=FACE_OUTER_BOUND('',#1647,.T.);
#1119=FACE_OUTER_BOUND('',#1648,.T.);
#1120=FACE_OUTER_BOUND('',#1649,.T.);
#1121=FACE_OUTER_BOUND('',#1650,.T.);
#1122=FACE_OUTER_BOUND('',#1651,.T.);
#1123=FACE_OUTER_BOUND('',#1652,.T.);
#1124=FACE_OUTER_BOUND('',#1654,.T.);
#1125=FACE_OUTER_BOUND('',#1655,.T.);
#1126=FACE_OUTER_BOUND('',#1657,.T.);
#1127=FACE_OUTER_BOUND('',#1658,.T.);
#1128=FACE_OUTER_BOUND('',#1659,.T.);
#1129=FACE_OUTER_BOUND('',#1661,.T.);
#1130=FACE_OUTER_BOUND('',#1662,.T.);
#1131=FACE_OUTER_BOUND('',#1664,.T.);
#1132=FACE_OUTER_BOUND('',#1665,.T.);
#1133=FACE_OUTER_BOUND('',#1667,.T.);
#1134=FACE_OUTER_BOUND('',#1668,.T.);
#1135=FACE_OUTER_BOUND('',#1670,.T.);
#1136=FACE_OUTER_BOUND('',#1671,.T.);
#1137=FACE_OUTER_BOUND('',#1673,.T.);
#1138=FACE_OUTER_BOUND('',#1675,.T.);
#1139=FACE_OUTER_BOUND('',#1676,.T.);
#1140=FACE_OUTER_BOUND('',#1677,.T.);
#1141=FACE_OUTER_BOUND('',#1678,.T.);
#1142=FACE_OUTER_BOUND('',#1679,.T.);
#1143=FACE_OUTER_BOUND('',#1680,.T.);
#1144=FACE_OUTER_BOUND('',#1681,.T.);
#1145=FACE_OUTER_BOUND('',#1682,.T.);
#1146=FACE_OUTER_BOUND('',#1684,.T.);
#1147=FACE_OUTER_BOUND('',#1685,.T.);
#1148=FACE_OUTER_BOUND('',#1686,.T.);
#1149=FACE_OUTER_BOUND('',#1687,.T.);
#1150=FACE_OUTER_BOUND('',#1689,.T.);
#1151=FACE_OUTER_BOUND('',#1690,.T.);
#1152=FACE_OUTER_BOUND('',#1691,.T.);
#1153=FACE_OUTER_BOUND('',#1692,.T.);
#1154=FACE_OUTER_BOUND('',#1693,.T.);
#1155=FACE_OUTER_BOUND('',#1694,.T.);
#1156=FACE_OUTER_BOUND('',#1696,.T.);
#1157=FACE_OUTER_BOUND('',#1697,.T.);
#1158=FACE_OUTER_BOUND('',#1698,.T.);
#1159=FACE_OUTER_BOUND('',#1699,.T.);
#1160=FACE_OUTER_BOUND('',#1700,.T.);
#1161=FACE_OUTER_BOUND('',#1701,.T.);
#1162=FACE_OUTER_BOUND('',#1702,.T.);
#1163=FACE_OUTER_BOUND('',#1703,.T.);
#1164=FACE_OUTER_BOUND('',#1704,.T.);
#1165=FACE_OUTER_BOUND('',#1705,.T.);
#1166=FACE_OUTER_BOUND('',#1706,.T.);
#1167=FACE_OUTER_BOUND('',#1707,.T.);
#1168=EDGE_LOOP('',(#4068,#4069,#4070,#4071));
#1169=EDGE_LOOP('',(#4072,#4073,#4074,#4075));
#1170=EDGE_LOOP('',(#4076,#4077,#4078,#4079));
#1171=EDGE_LOOP('',(#4080,#4081,#4082,#4083));
#1172=EDGE_LOOP('',(#4084,#4085,#4086,#4087));
#1173=EDGE_LOOP('',(#4088,#4089,#4090,#4091));
#1174=EDGE_LOOP('',(#4092,#4093,#4094,#4095));
#1175=EDGE_LOOP('',(#4096,#4097,#4098,#4099));
#1176=EDGE_LOOP('',(#4100,#4101,#4102,#4103));
#1177=EDGE_LOOP('',(#4104));
#1178=EDGE_LOOP('',(#4105));
#1179=EDGE_LOOP('',(#4106));
#1180=EDGE_LOOP('',(#4107));
#1181=EDGE_LOOP('',(#4108,#4109,#4110,#4111));
#1182=EDGE_LOOP('',(#4112));
#1183=EDGE_LOOP('',(#4113));
#1184=EDGE_LOOP('',(#4114));
#1185=EDGE_LOOP('',(#4115));
#1186=EDGE_LOOP('',(#4116,#4117,#4118,#4119));
#1187=EDGE_LOOP('',(#4120));
#1188=EDGE_LOOP('',(#4121,#4122,#4123,#4124));
#1189=EDGE_LOOP('',(#4125));
#1190=EDGE_LOOP('',(#4126));
#1191=EDGE_LOOP('',(#4127,#4128,#4129,#4130));
#1192=EDGE_LOOP('',(#4131));
#1193=EDGE_LOOP('',(#4132));
#1194=EDGE_LOOP('',(#4133,#4134,#4135,#4136));
#1195=EDGE_LOOP('',(#4137,#4138,#4139,#4140));
#1196=EDGE_LOOP('',(#4141,#4142,#4143,#4144));
#1197=EDGE_LOOP('',(#4145,#4146,#4147,#4148));
#1198=EDGE_LOOP('',(#4149,#4150,#4151,#4152));
#1199=EDGE_LOOP('',(#4153,#4154,#4155,#4156));
#1200=EDGE_LOOP('',(#4157,#4158,#4159,#4160));
#1201=EDGE_LOOP('',(#4161));
#1202=EDGE_LOOP('',(#4162));
#1203=EDGE_LOOP('',(#4163));
#1204=EDGE_LOOP('',(#4164,#4165,#4166,#4167));
#1205=EDGE_LOOP('',(#4168));
#1206=EDGE_LOOP('',(#4169));
#1207=EDGE_LOOP('',(#4170,#4171,#4172,#4173));
#1208=EDGE_LOOP('',(#4174));
#1209=EDGE_LOOP('',(#4175,#4176,#4177,#4178));
#1210=EDGE_LOOP('',(#4179));
#1211=EDGE_LOOP('',(#4180));
#1212=EDGE_LOOP('',(#4181,#4182,#4183,#4184));
#1213=EDGE_LOOP('',(#4185));
#1214=EDGE_LOOP('',(#4186));
#1215=EDGE_LOOP('',(#4187,#4188,#4189,#4190));
#1216=EDGE_LOOP('',(#4191,#4192,#4193,#4194));
#1217=EDGE_LOOP('',(#4195,#4196,#4197,#4198));
#1218=EDGE_LOOP('',(#4199,#4200,#4201,#4202));
#1219=EDGE_LOOP('',(#4203,#4204,#4205,#4206));
#1220=EDGE_LOOP('',(#4207,#4208,#4209,#4210));
#1221=EDGE_LOOP('',(#4211,#4212,#4213,#4214));
#1222=EDGE_LOOP('',(#4215));
#1223=EDGE_LOOP('',(#4216));
#1224=EDGE_LOOP('',(#4217));
#1225=EDGE_LOOP('',(#4218,#4219,#4220,#4221));
#1226=EDGE_LOOP('',(#4222));
#1227=EDGE_LOOP('',(#4223));
#1228=EDGE_LOOP('',(#4224,#4225));
#1229=EDGE_LOOP('',(#4226,#4227));
#1230=EDGE_LOOP('',(#4228,#4229));
#1231=EDGE_LOOP('',(#4230,#4231,#4232,#4233,#4234,#4235,#4236,#4237,#4238,
#4239,#4240,#4241,#4242,#4243,#4244));
#1232=EDGE_LOOP('',(#4245,#4246,#4247));
#1233=EDGE_LOOP('',(#4248,#4249,#4250));
#1234=EDGE_LOOP('',(#4251,#4252));
#1235=EDGE_LOOP('',(#4253,#4254));
#1236=EDGE_LOOP('',(#4255,#4256));
#1237=EDGE_LOOP('',(#4257,#4258));
#1238=EDGE_LOOP('',(#4259,#4260,#4261));
#1239=EDGE_LOOP('',(#4262,#4263,#4264,#4265,#4266,#4267,#4268,#4269,#4270));
#1240=EDGE_LOOP('',(#4271,#4272,#4273));
#1241=EDGE_LOOP('',(#4274,#4275));
#1242=EDGE_LOOP('',(#4276,#4277,#4278,#4279));
#1243=EDGE_LOOP('',(#4280));
#1244=EDGE_LOOP('',(#4281));
#1245=EDGE_LOOP('',(#4282,#4283,#4284,#4285,#4286,#4287));
#1246=EDGE_LOOP('',(#4288,#4289,#4290,#4291));
#1247=EDGE_LOOP('',(#4292));
#1248=EDGE_LOOP('',(#4293));
#1249=EDGE_LOOP('',(#4294,#4295,#4296,#4297,#4298));
#1250=EDGE_LOOP('',(#4299,#4300,#4301,#4302));
#1251=EDGE_LOOP('',(#4303));
#1252=EDGE_LOOP('',(#4304));
#1253=EDGE_LOOP('',(#4305,#4306,#4307,#4308,#4309,#4310));
#1254=EDGE_LOOP('',(#4311,#4312,#4313,#4314));
#1255=EDGE_LOOP('',(#4315));
#1256=EDGE_LOOP('',(#4316));
#1257=EDGE_LOOP('',(#4317,#4318,#4319,#4320,#4321));
#1258=EDGE_LOOP('',(#4322,#4323,#4324,#4325));
#1259=EDGE_LOOP('',(#4326));
#1260=EDGE_LOOP('',(#4327));
#1261=EDGE_LOOP('',(#4328,#4329,#4330,#4331,#4332,#4333));
#1262=EDGE_LOOP('',(#4334,#4335,#4336,#4337));
#1263=EDGE_LOOP('',(#4338));
#1264=EDGE_LOOP('',(#4339));
#1265=EDGE_LOOP('',(#4340,#4341,#4342,#4343,#4344));
#1266=EDGE_LOOP('',(#4345,#4346,#4347,#4348));
#1267=EDGE_LOOP('',(#4349));
#1268=EDGE_LOOP('',(#4350));
#1269=EDGE_LOOP('',(#4351,#4352,#4353,#4354,#4355,#4356));
#1270=EDGE_LOOP('',(#4357,#4358,#4359,#4360));
#1271=EDGE_LOOP('',(#4361));
#1272=EDGE_LOOP('',(#4362));
#1273=EDGE_LOOP('',(#4363,#4364,#4365,#4366,#4367));
#1274=EDGE_LOOP('',(#4368,#4369,#4370,#4371));
#1275=EDGE_LOOP('',(#4372));
#1276=EDGE_LOOP('',(#4373));
#1277=EDGE_LOOP('',(#4374,#4375,#4376,#4377,#4378,#4379,#4380,#4381,#4382,
#4383,#4384,#4385,#4386,#4387,#4388,#4389,#4390,#4391,#4392,#4393,#4394,
#4395,#4396,#4397,#4398,#4399,#4400,#4401,#4402,#4403,#4404,#4405,#4406));
#1278=EDGE_LOOP('',(#4407,#4408));
#1279=EDGE_LOOP('',(#4409,#4410));
#1280=EDGE_LOOP('',(#4411,#4412));
#1281=EDGE_LOOP('',(#4413,#4414));
#1282=EDGE_LOOP('',(#4415,#4416,#4417,#4418));
#1283=EDGE_LOOP('',(#4419));
#1284=EDGE_LOOP('',(#4420));
#1285=EDGE_LOOP('',(#4421,#4422,#4423,#4424));
#1286=EDGE_LOOP('',(#4425));
#1287=EDGE_LOOP('',(#4426));
#1288=EDGE_LOOP('',(#4427,#4428,#4429,#4430));
#1289=EDGE_LOOP('',(#4431));
#1290=EDGE_LOOP('',(#4432));
#1291=EDGE_LOOP('',(#4433,#4434,#4435,#4436));
#1292=EDGE_LOOP('',(#4437));
#1293=EDGE_LOOP('',(#4438));
#1294=EDGE_LOOP('',(#4439,#4440,#4441,#4442));
#1295=EDGE_LOOP('',(#4443,#4444,#4445,#4446));
#1296=EDGE_LOOP('',(#4447,#4448,#4449,#4450));
#1297=EDGE_LOOP('',(#4451,#4452,#4453,#4454));
#1298=EDGE_LOOP('',(#4455,#4456,#4457,#4458));
#1299=EDGE_LOOP('',(#4459,#4460,#4461,#4462));
#1300=EDGE_LOOP('',(#4463));
#1301=EDGE_LOOP('',(#4464,#4465,#4466,#4467));
#1302=EDGE_LOOP('',(#4468));
#1303=EDGE_LOOP('',(#4469));
#1304=EDGE_LOOP('',(#4470));
#1305=EDGE_LOOP('',(#4471));
#1306=EDGE_LOOP('',(#4472,#4473,#4474,#4475));
#1307=EDGE_LOOP('',(#4476));
#1308=EDGE_LOOP('',(#4477,#4478,#4479,#4480));
#1309=EDGE_LOOP('',(#4481));
#1310=EDGE_LOOP('',(#4482));
#1311=EDGE_LOOP('',(#4483));
#1312=EDGE_LOOP('',(#4484));
#1313=EDGE_LOOP('',(#4485));
#1314=EDGE_LOOP('',(#4486));
#1315=EDGE_LOOP('',(#4487));
#1316=EDGE_LOOP('',(#4488));
#1317=EDGE_LOOP('',(#4489));
#1318=EDGE_LOOP('',(#4490,#4491,#4492,#4493));
#1319=EDGE_LOOP('',(#4494));
#1320=EDGE_LOOP('',(#4495));
#1321=EDGE_LOOP('',(#4496));
#1322=EDGE_LOOP('',(#4497));
#1323=EDGE_LOOP('',(#4498,#4499,#4500,#4501));
#1324=EDGE_LOOP('',(#4502,#4503,#4504,#4505));
#1325=EDGE_LOOP('',(#4506));
#1326=EDGE_LOOP('',(#4507));
#1327=EDGE_LOOP('',(#4508));
#1328=EDGE_LOOP('',(#4509));
#1329=EDGE_LOOP('',(#4510));
#1330=EDGE_LOOP('',(#4511));
#1331=EDGE_LOOP('',(#4512,#4513,#4514,#4515));
#1332=EDGE_LOOP('',(#4516));
#1333=EDGE_LOOP('',(#4517));
#1334=EDGE_LOOP('',(#4518));
#1335=EDGE_LOOP('',(#4519,#4520,#4521,#4522));
#1336=EDGE_LOOP('',(#4523,#4524,#4525,#4526));
#1337=EDGE_LOOP('',(#4527));
#1338=EDGE_LOOP('',(#4528,#4529,#4530,#4531));
#1339=EDGE_LOOP('',(#4532,#4533,#4534,#4535));
#1340=EDGE_LOOP('',(#4536));
#1341=EDGE_LOOP('',(#4537));
#1342=EDGE_LOOP('',(#4538));
#1343=EDGE_LOOP('',(#4539));
#1344=EDGE_LOOP('',(#4540,#4541,#4542,#4543));
#1345=EDGE_LOOP('',(#4544,#4545,#4546,#4547));
#1346=EDGE_LOOP('',(#4548));
#1347=EDGE_LOOP('',(#4549));
#1348=EDGE_LOOP('',(#4550));
#1349=EDGE_LOOP('',(#4551));
#1350=EDGE_LOOP('',(#4552));
#1351=EDGE_LOOP('',(#4553));
#1352=EDGE_LOOP('',(#4554,#4555,#4556,#4557));
#1353=EDGE_LOOP('',(#4558));
#1354=EDGE_LOOP('',(#4559));
#1355=EDGE_LOOP('',(#4560));
#1356=EDGE_LOOP('',(#4561,#4562,#4563,#4564));
#1357=EDGE_LOOP('',(#4565,#4566,#4567,#4568));
#1358=EDGE_LOOP('',(#4569));
#1359=EDGE_LOOP('',(#4570,#4571,#4572,#4573));
#1360=EDGE_LOOP('',(#4574,#4575,#4576,#4577));
#1361=EDGE_LOOP('',(#4578));
#1362=EDGE_LOOP('',(#4579));
#1363=EDGE_LOOP('',(#4580));
#1364=EDGE_LOOP('',(#4581));
#1365=EDGE_LOOP('',(#4582,#4583,#4584,#4585));
#1366=EDGE_LOOP('',(#4586,#4587,#4588,#4589));
#1367=EDGE_LOOP('',(#4590));
#1368=EDGE_LOOP('',(#4591));
#1369=EDGE_LOOP('',(#4592));
#1370=EDGE_LOOP('',(#4593));
#1371=EDGE_LOOP('',(#4594));
#1372=EDGE_LOOP('',(#4595));
#1373=EDGE_LOOP('',(#4596,#4597,#4598,#4599));
#1374=EDGE_LOOP('',(#4600));
#1375=EDGE_LOOP('',(#4601));
#1376=EDGE_LOOP('',(#4602));
#1377=EDGE_LOOP('',(#4603,#4604,#4605,#4606));
#1378=EDGE_LOOP('',(#4607,#4608,#4609,#4610));
#1379=EDGE_LOOP('',(#4611));
#1380=EDGE_LOOP('',(#4612,#4613,#4614,#4615));
#1381=EDGE_LOOP('',(#4616,#4617,#4618,#4619));
#1382=EDGE_LOOP('',(#4620));
#1383=EDGE_LOOP('',(#4621));
#1384=EDGE_LOOP('',(#4622));
#1385=EDGE_LOOP('',(#4623));
#1386=EDGE_LOOP('',(#4624,#4625,#4626,#4627));
#1387=EDGE_LOOP('',(#4628,#4629,#4630,#4631));
#1388=EDGE_LOOP('',(#4632));
#1389=EDGE_LOOP('',(#4633));
#1390=EDGE_LOOP('',(#4634));
#1391=EDGE_LOOP('',(#4635));
#1392=EDGE_LOOP('',(#4636));
#1393=EDGE_LOOP('',(#4637));
#1394=EDGE_LOOP('',(#4638,#4639,#4640,#4641));
#1395=EDGE_LOOP('',(#4642));
#1396=EDGE_LOOP('',(#4643));
#1397=EDGE_LOOP('',(#4644));
#1398=EDGE_LOOP('',(#4645,#4646,#4647,#4648));
#1399=EDGE_LOOP('',(#4649,#4650,#4651,#4652));
#1400=EDGE_LOOP('',(#4653));
#1401=EDGE_LOOP('',(#4654,#4655,#4656,#4657));
#1402=EDGE_LOOP('',(#4658,#4659,#4660,#4661));
#1403=EDGE_LOOP('',(#4662));
#1404=EDGE_LOOP('',(#4663));
#1405=EDGE_LOOP('',(#4664));
#1406=EDGE_LOOP('',(#4665));
#1407=EDGE_LOOP('',(#4666,#4667,#4668,#4669));
#1408=EDGE_LOOP('',(#4670));
#1409=EDGE_LOOP('',(#4671));
#1410=EDGE_LOOP('',(#4672,#4673,#4674,#4675));
#1411=EDGE_LOOP('',(#4676));
#1412=EDGE_LOOP('',(#4677));
#1413=EDGE_LOOP('',(#4678,#4679,#4680,#4681));
#1414=EDGE_LOOP('',(#4682));
#1415=EDGE_LOOP('',(#4683,#4684,#4685,#4686));
#1416=EDGE_LOOP('',(#4687));
#1417=EDGE_LOOP('',(#4688,#4689,#4690,#4691));
#1418=EDGE_LOOP('',(#4692));
#1419=EDGE_LOOP('',(#4693,#4694,#4695,#4696));
#1420=EDGE_LOOP('',(#4697));
#1421=EDGE_LOOP('',(#4698,#4699,#4700,#4701));
#1422=EDGE_LOOP('',(#4702,#4703,#4704,#4705));
#1423=EDGE_LOOP('',(#4706,#4707,#4708,#4709));
#1424=EDGE_LOOP('',(#4710,#4711,#4712,#4713));
#1425=EDGE_LOOP('',(#4714,#4715,#4716,#4717));
#1426=EDGE_LOOP('',(#4718,#4719,#4720));
#1427=EDGE_LOOP('',(#4721,#4722,#4723));
#1428=EDGE_LOOP('',(#4724,#4725,#4726));
#1429=EDGE_LOOP('',(#4727,#4728,#4729,#4730));
#1430=EDGE_LOOP('',(#4731,#4732,#4733));
#1431=EDGE_LOOP('',(#4734,#4735,#4736,#4737,#4738,#4739,#4740,#4741));
#1432=EDGE_LOOP('',(#4742));
#1433=EDGE_LOOP('',(#4743));
#1434=EDGE_LOOP('',(#4744,#4745,#4746,#4747));
#1435=EDGE_LOOP('',(#4748,#4749,#4750,#4751,#4752));
#1436=EDGE_LOOP('',(#4753,#4754,#4755,#4756));
#1437=EDGE_LOOP('',(#4757,#4758,#4759,#4760,#4761));
#1438=EDGE_LOOP('',(#4762,#4763,#4764,#4765,#4766,#4767,#4768,#4769));
#1439=EDGE_LOOP('',(#4770));
#1440=EDGE_LOOP('',(#4771));
#1441=EDGE_LOOP('',(#4772,#4773,#4774,#4775));
#1442=EDGE_LOOP('',(#4776,#4777,#4778,#4779,#4780,#4781,#4782,#4783,#4784,
#4785,#4786,#4787,#4788,#4789,#4790,#4791));
#1443=EDGE_LOOP('',(#4792));
#1444=EDGE_LOOP('',(#4793));
#1445=EDGE_LOOP('',(#4794));
#1446=EDGE_LOOP('',(#4795));
#1447=EDGE_LOOP('',(#4796));
#1448=EDGE_LOOP('',(#4797));
#1449=EDGE_LOOP('',(#4798,#4799,#4800,#4801));
#1450=EDGE_LOOP('',(#4802,#4803,#4804,#4805));
#1451=EDGE_LOOP('',(#4806));
#1452=EDGE_LOOP('',(#4807));
#1453=EDGE_LOOP('',(#4808));
#1454=EDGE_LOOP('',(#4809));
#1455=EDGE_LOOP('',(#4810));
#1456=EDGE_LOOP('',(#4811));
#1457=EDGE_LOOP('',(#4812));
#1458=EDGE_LOOP('',(#4813));
#1459=EDGE_LOOP('',(#4814,#4815,#4816,#4817));
#1460=EDGE_LOOP('',(#4818,#4819,#4820,#4821));
#1461=EDGE_LOOP('',(#4822,#4823,#4824,#4825));
#1462=EDGE_LOOP('',(#4826,#4827,#4828,#4829));
#1463=EDGE_LOOP('',(#4830,#4831,#4832,#4833));
#1464=EDGE_LOOP('',(#4834,#4835,#4836,#4837));
#1465=EDGE_LOOP('',(#4838,#4839,#4840,#4841));
#1466=EDGE_LOOP('',(#4842,#4843,#4844,#4845));
#1467=EDGE_LOOP('',(#4846,#4847,#4848,#4849));
#1468=EDGE_LOOP('',(#4850,#4851,#4852,#4853));
#1469=EDGE_LOOP('',(#4854));
#1470=EDGE_LOOP('',(#4855));
#1471=EDGE_LOOP('',(#4856));
#1472=EDGE_LOOP('',(#4857));
#1473=EDGE_LOOP('',(#4858,#4859,#4860,#4861));
#1474=EDGE_LOOP('',(#4862,#4863,#4864,#4865));
#1475=EDGE_LOOP('',(#4866,#4867,#4868,#4869));
#1476=EDGE_LOOP('',(#4870));
#1477=EDGE_LOOP('',(#4871));
#1478=EDGE_LOOP('',(#4872));
#1479=EDGE_LOOP('',(#4873));
#1480=EDGE_LOOP('',(#4874,#4875,#4876,#4877));
#1481=EDGE_LOOP('',(#4878,#4879,#4880,#4881));
#1482=EDGE_LOOP('',(#4882,#4883,#4884,#4885));
#1483=EDGE_LOOP('',(#4886,#4887,#4888,#4889));
#1484=EDGE_LOOP('',(#4890,#4891,#4892,#4893));
#1485=EDGE_LOOP('',(#4894,#4895,#4896,#4897));
#1486=EDGE_LOOP('',(#4898,#4899,#4900,#4901));
#1487=EDGE_LOOP('',(#4902,#4903,#4904,#4905));
#1488=EDGE_LOOP('',(#4906));
#1489=EDGE_LOOP('',(#4907));
#1490=EDGE_LOOP('',(#4908));
#1491=EDGE_LOOP('',(#4909));
#1492=EDGE_LOOP('',(#4910,#4911,#4912,#4913));
#1493=EDGE_LOOP('',(#4914,#4915,#4916,#4917));
#1494=EDGE_LOOP('',(#4918));
#1495=EDGE_LOOP('',(#4919));
#1496=EDGE_LOOP('',(#4920));
#1497=EDGE_LOOP('',(#4921));
#1498=EDGE_LOOP('',(#4922,#4923,#4924,#4925));
#1499=EDGE_LOOP('',(#4926,#4927,#4928,#4929));
#1500=EDGE_LOOP('',(#4930,#4931,#4932,#4933));
#1501=EDGE_LOOP('',(#4934,#4935,#4936,#4937));
#1502=EDGE_LOOP('',(#4938,#4939,#4940,#4941));
#1503=EDGE_LOOP('',(#4942,#4943,#4944,#4945));
#1504=EDGE_LOOP('',(#4946,#4947,#4948,#4949));
#1505=EDGE_LOOP('',(#4950,#4951,#4952,#4953));
#1506=EDGE_LOOP('',(#4954,#4955,#4956,#4957));
#1507=EDGE_LOOP('',(#4958,#4959,#4960,#4961));
#1508=EDGE_LOOP('',(#4962,#4963,#4964,#4965));
#1509=EDGE_LOOP('',(#4966,#4967,#4968,#4969));
#1510=EDGE_LOOP('',(#4970,#4971,#4972,#4973));
#1511=EDGE_LOOP('',(#4974));
#1512=EDGE_LOOP('',(#4975));
#1513=EDGE_LOOP('',(#4976));
#1514=EDGE_LOOP('',(#4977));
#1515=EDGE_LOOP('',(#4978,#4979,#4980,#4981));
#1516=EDGE_LOOP('',(#4982,#4983,#4984,#4985));
#1517=EDGE_LOOP('',(#4986,#4987,#4988,#4989));
#1518=EDGE_LOOP('',(#4990));
#1519=EDGE_LOOP('',(#4991));
#1520=EDGE_LOOP('',(#4992));
#1521=EDGE_LOOP('',(#4993));
#1522=EDGE_LOOP('',(#4994,#4995,#4996,#4997));
#1523=EDGE_LOOP('',(#4998,#4999,#5000,#5001));
#1524=EDGE_LOOP('',(#5002,#5003,#5004,#5005));
#1525=EDGE_LOOP('',(#5006,#5007,#5008,#5009));
#1526=EDGE_LOOP('',(#5010,#5011,#5012,#5013));
#1527=EDGE_LOOP('',(#5014,#5015,#5016,#5017));
#1528=EDGE_LOOP('',(#5018,#5019));
#1529=EDGE_LOOP('',(#5020,#5021,#5022));
#1530=EDGE_LOOP('',(#5023));
#1531=EDGE_LOOP('',(#5024));
#1532=EDGE_LOOP('',(#5025,#5026,#5027,#5028,#5029,#5030,#5031,#5032,#5033,
#5034,#5035,#5036));
#1533=EDGE_LOOP('',(#5037,#5038,#5039,#5040));
#1534=EDGE_LOOP('',(#5041));
#1535=EDGE_LOOP('',(#5042,#5043,#5044,#5045));
#1536=EDGE_LOOP('',(#5046,#5047,#5048,#5049));
#1537=EDGE_LOOP('',(#5050,#5051,#5052,#5053));
#1538=EDGE_LOOP('',(#5054,#5055));
#1539=EDGE_LOOP('',(#5056,#5057,#5058));
#1540=EDGE_LOOP('',(#5059));
#1541=EDGE_LOOP('',(#5060));
#1542=EDGE_LOOP('',(#5061,#5062,#5063,#5064,#5065,#5066,#5067,#5068,#5069,
#5070,#5071,#5072));
#1543=EDGE_LOOP('',(#5073,#5074,#5075,#5076));
#1544=EDGE_LOOP('',(#5077));
#1545=EDGE_LOOP('',(#5078,#5079,#5080,#5081));
#1546=EDGE_LOOP('',(#5082,#5083,#5084,#5085));
#1547=EDGE_LOOP('',(#5086,#5087,#5088,#5089));
#1548=EDGE_LOOP('',(#5090,#5091));
#1549=EDGE_LOOP('',(#5092,#5093,#5094));
#1550=EDGE_LOOP('',(#5095));
#1551=EDGE_LOOP('',(#5096));
#1552=EDGE_LOOP('',(#5097,#5098,#5099,#5100,#5101,#5102,#5103,#5104,#5105,
#5106,#5107,#5108));
#1553=EDGE_LOOP('',(#5109,#5110,#5111,#5112));
#1554=EDGE_LOOP('',(#5113));
#1555=EDGE_LOOP('',(#5114,#5115,#5116,#5117));
#1556=EDGE_LOOP('',(#5118,#5119,#5120,#5121));
#1557=EDGE_LOOP('',(#5122,#5123,#5124,#5125));
#1558=EDGE_LOOP('',(#5126,#5127));
#1559=EDGE_LOOP('',(#5128,#5129,#5130));
#1560=EDGE_LOOP('',(#5131));
#1561=EDGE_LOOP('',(#5132));
#1562=EDGE_LOOP('',(#5133,#5134,#5135,#5136,#5137,#5138,#5139,#5140,#5141,
#5142,#5143,#5144));
#1563=EDGE_LOOP('',(#5145,#5146,#5147,#5148));
#1564=EDGE_LOOP('',(#5149));
#1565=EDGE_LOOP('',(#5150,#5151,#5152,#5153));
#1566=EDGE_LOOP('',(#5154,#5155,#5156,#5157));
#1567=EDGE_LOOP('',(#5158,#5159,#5160,#5161));
#1568=EDGE_LOOP('',(#5162,#5163,#5164,#5165));
#1569=EDGE_LOOP('',(#5166,#5167,#5168,#5169));
#1570=EDGE_LOOP('',(#5170,#5171,#5172,#5173));
#1571=EDGE_LOOP('',(#5174));
#1572=EDGE_LOOP('',(#5175));
#1573=EDGE_LOOP('',(#5176));
#1574=EDGE_LOOP('',(#5177));
#1575=EDGE_LOOP('',(#5178));
#1576=EDGE_LOOP('',(#5179));
#1577=EDGE_LOOP('',(#5180));
#1578=EDGE_LOOP('',(#5181));
#1579=EDGE_LOOP('',(#5182));
#1580=EDGE_LOOP('',(#5183));
#1581=EDGE_LOOP('',(#5184));
#1582=EDGE_LOOP('',(#5185));
#1583=EDGE_LOOP('',(#5186,#5187,#5188,#5189));
#1584=EDGE_LOOP('',(#5190,#5191,#5192,#5193));
#1585=EDGE_LOOP('',(#5194,#5195,#5196,#5197));
#1586=EDGE_LOOP('',(#5198,#5199,#5200,#5201));
#1587=EDGE_LOOP('',(#5202,#5203,#5204,#5205));
#1588=EDGE_LOOP('',(#5206,#5207,#5208,#5209));
#1589=EDGE_LOOP('',(#5210));
#1590=EDGE_LOOP('',(#5211));
#1591=EDGE_LOOP('',(#5212));
#1592=EDGE_LOOP('',(#5213));
#1593=EDGE_LOOP('',(#5214));
#1594=EDGE_LOOP('',(#5215));
#1595=EDGE_LOOP('',(#5216));
#1596=EDGE_LOOP('',(#5217));
#1597=EDGE_LOOP('',(#5218));
#1598=EDGE_LOOP('',(#5219));
#1599=EDGE_LOOP('',(#5220));
#1600=EDGE_LOOP('',(#5221));
#1601=EDGE_LOOP('',(#5222,#5223,#5224,#5225));
#1602=EDGE_LOOP('',(#5226));
#1603=EDGE_LOOP('',(#5227));
#1604=EDGE_LOOP('',(#5228,#5229,#5230,#5231));
#1605=EDGE_LOOP('',(#5232));
#1606=EDGE_LOOP('',(#5233));
#1607=EDGE_LOOP('',(#5234,#5235,#5236,#5237));
#1608=EDGE_LOOP('',(#5238));
#1609=EDGE_LOOP('',(#5239));
#1610=EDGE_LOOP('',(#5240,#5241,#5242,#5243));
#1611=EDGE_LOOP('',(#5244,#5245,#5246,#5247));
#1612=EDGE_LOOP('',(#5248,#5249,#5250,#5251));
#1613=EDGE_LOOP('',(#5252,#5253,#5254,#5255));
#1614=EDGE_LOOP('',(#5256,#5257,#5258,#5259));
#1615=EDGE_LOOP('',(#5260,#5261,#5262,#5263));
#1616=EDGE_LOOP('',(#5264,#5265,#5266,#5267));
#1617=EDGE_LOOP('',(#5268,#5269,#5270,#5271));
#1618=EDGE_LOOP('',(#5272,#5273,#5274,#5275));
#1619=EDGE_LOOP('',(#5276,#5277,#5278,#5279));
#1620=EDGE_LOOP('',(#5280,#5281,#5282,#5283));
#1621=EDGE_LOOP('',(#5284,#5285,#5286,#5287));
#1622=EDGE_LOOP('',(#5288,#5289,#5290,#5291));
#1623=EDGE_LOOP('',(#5292,#5293,#5294,#5295));
#1624=EDGE_LOOP('',(#5296,#5297,#5298,#5299));
#1625=EDGE_LOOP('',(#5300,#5301,#5302,#5303));
#1626=EDGE_LOOP('',(#5304,#5305,#5306,#5307));
#1627=EDGE_LOOP('',(#5308,#5309,#5310,#5311));
#1628=EDGE_LOOP('',(#5312,#5313,#5314,#5315,#5316,#5317));
#1629=EDGE_LOOP('',(#5318,#5319,#5320,#5321,#5322,#5323));
#1630=EDGE_LOOP('',(#5324));
#1631=EDGE_LOOP('',(#5325));
#1632=EDGE_LOOP('',(#5326,#5327,#5328,#5329));
#1633=EDGE_LOOP('',(#5330,#5331,#5332,#5333));
#1634=EDGE_LOOP('',(#5334,#5335,#5336,#5337));
#1635=EDGE_LOOP('',(#5338));
#1636=EDGE_LOOP('',(#5339));
#1637=EDGE_LOOP('',(#5340,#5341,#5342,#5343));
#1638=EDGE_LOOP('',(#5344,#5345,#5346,#5347));
#1639=EDGE_LOOP('',(#5348,#5349,#5350,#5351));
#1640=EDGE_LOOP('',(#5352));
#1641=EDGE_LOOP('',(#5353));
#1642=EDGE_LOOP('',(#5354,#5355,#5356,#5357,#5358,#5359));
#1643=EDGE_LOOP('',(#5360));
#1644=EDGE_LOOP('',(#5361,#5362,#5363,#5364,#5365,#5366));
#1645=EDGE_LOOP('',(#5367));
#1646=EDGE_LOOP('',(#5368,#5369,#5370,#5371));
#1647=EDGE_LOOP('',(#5372,#5373,#5374,#5375));
#1648=EDGE_LOOP('',(#5376,#5377,#5378,#5379));
#1649=EDGE_LOOP('',(#5380,#5381,#5382,#5383));
#1650=EDGE_LOOP('',(#5384,#5385,#5386,#5387));
#1651=EDGE_LOOP('',(#5388,#5389,#5390,#5391));
#1652=EDGE_LOOP('',(#5392));
#1653=EDGE_LOOP('',(#5393));
#1654=EDGE_LOOP('',(#5394,#5395,#5396,#5397));
#1655=EDGE_LOOP('',(#5398));
#1656=EDGE_LOOP('',(#5399));
#1657=EDGE_LOOP('',(#5400,#5401,#5402,#5403));
#1658=EDGE_LOOP('',(#5404,#5405,#5406,#5407));
#1659=EDGE_LOOP('',(#5408));
#1660=EDGE_LOOP('',(#5409));
#1661=EDGE_LOOP('',(#5410,#5411,#5412,#5413));
#1662=EDGE_LOOP('',(#5414));
#1663=EDGE_LOOP('',(#5415));
#1664=EDGE_LOOP('',(#5416,#5417,#5418,#5419));
#1665=EDGE_LOOP('',(#5420));
#1666=EDGE_LOOP('',(#5421));
#1667=EDGE_LOOP('',(#5422,#5423,#5424,#5425));
#1668=EDGE_LOOP('',(#5426));
#1669=EDGE_LOOP('',(#5427));
#1670=EDGE_LOOP('',(#5428,#5429,#5430,#5431));
#1671=EDGE_LOOP('',(#5432,#5433,#5434,#5435,#5436,#5437));
#1672=EDGE_LOOP('',(#5438));
#1673=EDGE_LOOP('',(#5439,#5440,#5441,#5442,#5443,#5444));
#1674=EDGE_LOOP('',(#5445));
#1675=EDGE_LOOP('',(#5446,#5447,#5448,#5449));
#1676=EDGE_LOOP('',(#5450,#5451,#5452,#5453));
#1677=EDGE_LOOP('',(#5454,#5455,#5456,#5457));
#1678=EDGE_LOOP('',(#5458,#5459,#5460,#5461));
#1679=EDGE_LOOP('',(#5462,#5463,#5464,#5465));
#1680=EDGE_LOOP('',(#5466,#5467,#5468,#5469));
#1681=EDGE_LOOP('',(#5470,#5471,#5472,#5473));
#1682=EDGE_LOOP('',(#5474));
#1683=EDGE_LOOP('',(#5475));
#1684=EDGE_LOOP('',(#5476,#5477,#5478,#5479));
#1685=EDGE_LOOP('',(#5480,#5481,#5482,#5483));
#1686=EDGE_LOOP('',(#5484,#5485,#5486,#5487));
#1687=EDGE_LOOP('',(#5488));
#1688=EDGE_LOOP('',(#5489));
#1689=EDGE_LOOP('',(#5490,#5491,#5492,#5493));
#1690=EDGE_LOOP('',(#5494));
#1691=EDGE_LOOP('',(#5495,#5496,#5497,#5498));
#1692=EDGE_LOOP('',(#5499,#5500,#5501,#5502));
#1693=EDGE_LOOP('',(#5503,#5504,#5505,#5506));
#1694=EDGE_LOOP('',(#5507));
#1695=EDGE_LOOP('',(#5508));
#1696=EDGE_LOOP('',(#5509,#5510,#5511,#5512));
#1697=EDGE_LOOP('',(#5513,#5514,#5515,#5516));
#1698=EDGE_LOOP('',(#5517,#5518,#5519,#5520));
#1699=EDGE_LOOP('',(#5521));
#1700=EDGE_LOOP('',(#5522,#5523,#5524,#5525));
#1701=EDGE_LOOP('',(#5526,#5527,#5528,#5529));
#1702=EDGE_LOOP('',(#5530,#5531,#5532,#5533));
#1703=EDGE_LOOP('',(#5534,#5535,#5536,#5537));
#1704=EDGE_LOOP('',(#5538,#5539,#5540,#5541));
#1705=EDGE_LOOP('',(#5542,#5543,#5544,#5545));
#1706=EDGE_LOOP('',(#5546,#5547,#5548,#5549,#5550,#5551));
#1707=EDGE_LOOP('',(#5552,#5553,#5554,#5555,#5556,#5557));
#1708=LINE('',#9198,#2127);
#1709=LINE('',#9204,#2128);
#1710=LINE('',#9210,#2129);
#1711=LINE('',#9216,#2130);
#1712=LINE('',#9221,#2131);
#1713=LINE('',#9223,#2132);
#1714=LINE('',#9225,#2133);
#1715=LINE('',#9226,#2134);
#1716=LINE('',#9229,#2135);
#1717=LINE('',#9231,#2136);
#1718=LINE('',#9232,#2137);
#1719=LINE('',#9235,#2138);
#1720=LINE('',#9237,#2139);
#1721=LINE('',#9238,#2140);
#1722=LINE('',#9240,#2141);
#1723=LINE('',#9241,#2142);
#1724=LINE('',#9249,#2143);
#1725=LINE('',#9256,#2144);
#1726=LINE('',#9265,#2145);
#1727=LINE('',#9273,#2146);
#1728=LINE('',#9277,#2147);
#1729=LINE('',#9281,#2148);
#1730=LINE('',#9283,#2149);
#1731=LINE('',#9285,#2150);
#1732=LINE('',#9286,#2151);
#1733=LINE('',#9289,#2152);
#1734=LINE('',#9291,#2153);
#1735=LINE('',#9292,#2154);
#1736=LINE('',#9295,#2155);
#1737=LINE('',#9297,#2156);
#1738=LINE('',#9298,#2157);
#1739=LINE('',#9300,#2158);
#1740=LINE('',#9301,#2159);
#1741=LINE('',#9309,#2160);
#1742=LINE('',#9316,#2161);
#1743=LINE('',#9325,#2162);
#1744=LINE('',#9333,#2163);
#1745=LINE('',#9337,#2164);
#1746=LINE('',#9341,#2165);
#1747=LINE('',#9343,#2166);
#1748=LINE('',#9345,#2167);
#1749=LINE('',#9346,#2168);
#1750=LINE('',#9349,#2169);
#1751=LINE('',#9351,#2170);
#1752=LINE('',#9352,#2171);
#1753=LINE('',#9355,#2172);
#1754=LINE('',#9357,#2173);
#1755=LINE('',#9358,#2174);
#1756=LINE('',#9360,#2175);
#1757=LINE('',#9361,#2176);
#1758=LINE('',#9368,#2177);
#1759=LINE('',#9372,#2178);
#1760=LINE('',#9377,#2179);
#1761=LINE('',#9381,#2180);
#1762=LINE('',#9383,#2181);
#1763=LINE('',#9389,#2182);
#1764=LINE('',#9473,#2183);
#1765=LINE('',#9475,#2184);
#1766=LINE('',#9483,#2185);
#1767=LINE('',#9492,#2186);
#1768=LINE('',#9520,#2187);
#1769=LINE('',#9544,#2188);
#1770=LINE('',#9551,#2189);
#1771=LINE('',#9593,#2190);
#1772=LINE('',#9621,#2191);
#1773=LINE('',#9645,#2192);
#1774=LINE('',#9652,#2193);
#1775=LINE('',#9694,#2194);
#1776=LINE('',#9722,#2195);
#1777=LINE('',#9746,#2196);
#1778=LINE('',#9753,#2197);
#1779=LINE('',#9795,#2198);
#1780=LINE('',#9823,#2199);
#1781=LINE('',#9847,#2200);
#1782=LINE('',#9854,#2201);
#1783=LINE('',#9896,#2202);
#1784=LINE('',#9902,#2203);
#1785=LINE('',#9903,#2204);
#1786=LINE('',#9904,#2205);
#1787=LINE('',#9905,#2206);
#1788=LINE('',#9906,#2207);
#1789=LINE('',#9908,#2208);
#1790=LINE('',#9914,#2209);
#1791=LINE('',#9923,#2210);
#1792=LINE('',#9932,#2211);
#1793=LINE('',#9941,#2212);
#1794=LINE('',#9949,#2213);
#1795=LINE('',#9953,#2214);
#1796=LINE('',#9957,#2215);
#1797=LINE('',#9961,#2216);
#1798=LINE('',#9965,#2217);
#1799=LINE('',#9967,#2218);
#1800=LINE('',#9969,#2219);
#1801=LINE('',#9970,#2220);
#1802=LINE('',#9973,#2221);
#1803=LINE('',#9975,#2222);
#1804=LINE('',#9976,#2223);
#1805=LINE('',#9979,#2224);
#1806=LINE('',#9981,#2225);
#1807=LINE('',#9982,#2226);
#1808=LINE('',#9984,#2227);
#1809=LINE('',#9985,#2228);
#1810=LINE('',#9993,#2229);
#1811=LINE('',#9999,#2230);
#1812=LINE('',#10012,#2231);
#1813=LINE('',#10020,#2232);
#1814=LINE('',#10023,#2233);
#1815=LINE('',#10031,#2234);
#1816=LINE('',#10037,#2235);
#1817=LINE('',#10046,#2236);
#1818=LINE('',#10052,#2237);
#1819=LINE('',#10065,#2238);
#1820=LINE('',#10073,#2239);
#1821=LINE('',#10076,#2240);
#1822=LINE('',#10084,#2241);
#1823=LINE('',#10090,#2242);
#1824=LINE('',#10099,#2243);
#1825=LINE('',#10105,#2244);
#1826=LINE('',#10118,#2245);
#1827=LINE('',#10126,#2246);
#1828=LINE('',#10129,#2247);
#1829=LINE('',#10137,#2248);
#1830=LINE('',#10143,#2249);
#1831=LINE('',#10152,#2250);
#1832=LINE('',#10158,#2251);
#1833=LINE('',#10171,#2252);
#1834=LINE('',#10179,#2253);
#1835=LINE('',#10182,#2254);
#1836=LINE('',#10190,#2255);
#1837=LINE('',#10196,#2256);
#1838=LINE('',#10205,#2257);
#1839=LINE('',#10214,#2258);
#1840=LINE('',#10223,#2259);
#1841=LINE('',#10230,#2260);
#1842=LINE('',#10237,#2261);
#1843=LINE('',#10244,#2262);
#1844=LINE('',#10251,#2263);
#1845=LINE('',#10290,#2264);
#1846=LINE('',#10329,#2265);
#1847=LINE('',#10368,#2266);
#1848=LINE('',#10406,#2267);
#1849=LINE('',#10408,#2268);
#1850=LINE('',#10410,#2269);
#1851=LINE('',#10411,#2270);
#1852=LINE('',#10417,#2271);
#1853=LINE('',#10418,#2272);
#1854=LINE('',#10424,#2273);
#1855=LINE('',#10425,#2274);
#1856=LINE('',#10428,#2275);
#1857=LINE('',#10430,#2276);
#1858=LINE('',#10431,#2277);
#1859=LINE('',#10434,#2278);
#1860=LINE('',#10437,#2279);
#1861=LINE('',#10439,#2280);
#1862=LINE('',#10441,#2281);
#1863=LINE('',#10443,#2282);
#1864=LINE('',#10444,#2283);
#1865=LINE('',#10448,#2284);
#1866=LINE('',#10449,#2285);
#1867=LINE('',#10450,#2286);
#1868=LINE('',#10455,#2287);
#1869=LINE('',#10456,#2288);
#1870=LINE('',#10459,#2289);
#1871=LINE('',#10461,#2290);
#1872=LINE('',#10462,#2291);
#1873=LINE('',#10465,#2292);
#1874=LINE('',#10467,#2293);
#1875=LINE('',#10468,#2294);
#1876=LINE('',#10473,#2295);
#1877=LINE('',#10478,#2296);
#1878=LINE('',#10480,#2297);
#1879=LINE('',#10487,#2298);
#1880=LINE('',#10496,#2299);
#1881=LINE('',#10502,#2300);
#1882=LINE('',#10508,#2301);
#1883=LINE('',#10514,#2302);
#1884=LINE('',#10519,#2303);
#1885=LINE('',#10521,#2304);
#1886=LINE('',#10523,#2305);
#1887=LINE('',#10524,#2306);
#1888=LINE('',#10527,#2307);
#1889=LINE('',#10529,#2308);
#1890=LINE('',#10530,#2309);
#1891=LINE('',#10533,#2310);
#1892=LINE('',#10535,#2311);
#1893=LINE('',#10536,#2312);
#1894=LINE('',#10538,#2313);
#1895=LINE('',#10539,#2314);
#1896=LINE('',#10543,#2315);
#1897=LINE('',#10545,#2316);
#1898=LINE('',#10547,#2317);
#1899=LINE('',#10548,#2318);
#1900=LINE('',#10551,#2319);
#1901=LINE('',#10553,#2320);
#1902=LINE('',#10554,#2321);
#1903=LINE('',#10557,#2322);
#1904=LINE('',#10559,#2323);
#1905=LINE('',#10560,#2324);
#1906=LINE('',#10562,#2325);
#1907=LINE('',#10563,#2326);
#1908=LINE('',#10571,#2327);
#1909=LINE('',#10577,#2328);
#1910=LINE('',#10583,#2329);
#1911=LINE('',#10589,#2330);
#1912=LINE('',#10594,#2331);
#1913=LINE('',#10596,#2332);
#1914=LINE('',#10598,#2333);
#1915=LINE('',#10599,#2334);
#1916=LINE('',#10602,#2335);
#1917=LINE('',#10604,#2336);
#1918=LINE('',#10605,#2337);
#1919=LINE('',#10608,#2338);
#1920=LINE('',#10610,#2339);
#1921=LINE('',#10611,#2340);
#1922=LINE('',#10613,#2341);
#1923=LINE('',#10614,#2342);
#1924=LINE('',#10622,#2343);
#1925=LINE('',#10628,#2344);
#1926=LINE('',#10634,#2345);
#1927=LINE('',#10640,#2346);
#1928=LINE('',#10645,#2347);
#1929=LINE('',#10647,#2348);
#1930=LINE('',#10649,#2349);
#1931=LINE('',#10650,#2350);
#1932=LINE('',#10653,#2351);
#1933=LINE('',#10655,#2352);
#1934=LINE('',#10656,#2353);
#1935=LINE('',#10659,#2354);
#1936=LINE('',#10661,#2355);
#1937=LINE('',#10662,#2356);
#1938=LINE('',#10664,#2357);
#1939=LINE('',#10665,#2358);
#1940=LINE('',#10669,#2359);
#1941=LINE('',#10671,#2360);
#1942=LINE('',#10673,#2361);
#1943=LINE('',#10674,#2362);
#1944=LINE('',#10677,#2363);
#1945=LINE('',#10679,#2364);
#1946=LINE('',#10680,#2365);
#1947=LINE('',#10683,#2366);
#1948=LINE('',#10685,#2367);
#1949=LINE('',#10686,#2368);
#1950=LINE('',#10688,#2369);
#1951=LINE('',#10689,#2370);
#1952=LINE('',#10696,#2371);
#1953=LINE('',#10698,#2372);
#1954=LINE('',#10700,#2373);
#1955=LINE('',#10701,#2374);
#1956=LINE('',#10705,#2375);
#1957=LINE('',#10707,#2376);
#1958=LINE('',#10709,#2377);
#1959=LINE('',#10710,#2378);
#1960=LINE('',#10726,#2379);
#1961=LINE('',#10730,#2380);
#1962=LINE('',#10736,#2381);
#1963=LINE('',#10738,#2382);
#1964=LINE('',#10740,#2383);
#1965=LINE('',#10741,#2384);
#1966=LINE('',#10745,#2385);
#1967=LINE('',#10747,#2386);
#1968=LINE('',#10749,#2387);
#1969=LINE('',#10750,#2388);
#1970=LINE('',#10766,#2389);
#1971=LINE('',#10770,#2390);
#1972=LINE('',#10776,#2391);
#1973=LINE('',#10778,#2392);
#1974=LINE('',#10780,#2393);
#1975=LINE('',#10781,#2394);
#1976=LINE('',#10785,#2395);
#1977=LINE('',#10787,#2396);
#1978=LINE('',#10789,#2397);
#1979=LINE('',#10790,#2398);
#1980=LINE('',#10806,#2399);
#1981=LINE('',#10810,#2400);
#1982=LINE('',#10816,#2401);
#1983=LINE('',#10818,#2402);
#1984=LINE('',#10820,#2403);
#1985=LINE('',#10821,#2404);
#1986=LINE('',#10825,#2405);
#1987=LINE('',#10827,#2406);
#1988=LINE('',#10829,#2407);
#1989=LINE('',#10830,#2408);
#1990=LINE('',#10846,#2409);
#1991=LINE('',#10850,#2410);
#1992=LINE('',#10857,#2411);
#1993=LINE('',#10863,#2412);
#1994=LINE('',#10869,#2413);
#1995=LINE('',#10875,#2414);
#1996=LINE('',#10881,#2415);
#1997=LINE('',#10887,#2416);
#1998=LINE('',#10896,#2417);
#1999=LINE('',#10902,#2418);
#2000=LINE('',#10908,#2419);
#2001=LINE('',#10914,#2420);
#2002=LINE('',#10920,#2421);
#2003=LINE('',#10926,#2422);
#2004=LINE('',#10935,#2423);
#2005=LINE('',#10945,#2424);
#2006=LINE('',#10949,#2425);
#2007=LINE('',#10956,#2426);
#2008=LINE('',#10958,#2427);
#2009=LINE('',#10960,#2428);
#2010=LINE('',#10961,#2429);
#2011=LINE('',#10964,#2430);
#2012=LINE('',#10966,#2431);
#2013=LINE('',#10967,#2432);
#2014=LINE('',#10970,#2433);
#2015=LINE('',#10972,#2434);
#2016=LINE('',#10973,#2435);
#2017=LINE('',#10975,#2436);
#2018=LINE('',#10976,#2437);
#2019=LINE('',#10983,#2438);
#2020=LINE('',#10985,#2439);
#2021=LINE('',#10987,#2440);
#2022=LINE('',#10988,#2441);
#2023=LINE('',#10991,#2442);
#2024=LINE('',#10993,#2443);
#2025=LINE('',#10994,#2444);
#2026=LINE('',#10997,#2445);
#2027=LINE('',#10999,#2446);
#2028=LINE('',#11000,#2447);
#2029=LINE('',#11002,#2448);
#2030=LINE('',#11003,#2449);
#2031=LINE('',#11010,#2450);
#2032=LINE('',#11012,#2451);
#2033=LINE('',#11014,#2452);
#2034=LINE('',#11015,#2453);
#2035=LINE('',#11018,#2454);
#2036=LINE('',#11020,#2455);
#2037=LINE('',#11021,#2456);
#2038=LINE('',#11024,#2457);
#2039=LINE('',#11026,#2458);
#2040=LINE('',#11027,#2459);
#2041=LINE('',#11030,#2460);
#2042=LINE('',#11032,#2461);
#2043=LINE('',#11033,#2462);
#2044=LINE('',#11036,#2463);
#2045=LINE('',#11038,#2464);
#2046=LINE('',#11039,#2465);
#2047=LINE('',#11041,#2466);
#2048=LINE('',#11042,#2467);
#2049=LINE('',#11054,#2468);
#2050=LINE('',#11058,#2469);
#2051=LINE('',#11062,#2470);
#2052=LINE('',#11069,#2471);
#2053=LINE('',#11071,#2472);
#2054=LINE('',#11078,#2473);
#2055=LINE('',#11086,#2474);
#2056=LINE('',#11088,#2475);
#2057=LINE('',#11090,#2476);
#2058=LINE('',#11092,#2477);
#2059=LINE('',#11094,#2478);
#2060=LINE('',#11095,#2479);
#2061=LINE('',#11101,#2480);
#2062=LINE('',#11103,#2481);
#2063=LINE('',#11105,#2482);
#2064=LINE('',#11107,#2483);
#2065=LINE('',#11109,#2484);
#2066=LINE('',#11110,#2485);
#2067=LINE('',#11114,#2486);
#2068=LINE('',#11115,#2487);
#2069=LINE('',#11117,#2488);
#2070=LINE('',#11119,#2489);
#2071=LINE('',#11121,#2490);
#2072=LINE('',#11123,#2491);
#2073=LINE('',#11130,#2492);
#2074=LINE('',#11136,#2493);
#2075=LINE('',#11140,#2494);
#2076=LINE('',#11145,#2495);
#2077=LINE('',#11155,#2496);
#2078=LINE('',#11162,#2497);
#2079=LINE('',#11167,#2498);
#2080=LINE('',#11174,#2499);
#2081=LINE('',#11176,#2500);
#2082=LINE('',#11178,#2501);
#2083=LINE('',#11180,#2502);
#2084=LINE('',#11182,#2503);
#2085=LINE('',#11183,#2504);
#2086=LINE('',#11189,#2505);
#2087=LINE('',#11191,#2506);
#2088=LINE('',#11193,#2507);
#2089=LINE('',#11195,#2508);
#2090=LINE('',#11197,#2509);
#2091=LINE('',#11198,#2510);
#2092=LINE('',#11202,#2511);
#2093=LINE('',#11203,#2512);
#2094=LINE('',#11205,#2513);
#2095=LINE('',#11207,#2514);
#2096=LINE('',#11209,#2515);
#2097=LINE('',#11211,#2516);
#2098=LINE('',#11215,#2517);
#2099=LINE('',#11223,#2518);
#2100=LINE('',#11227,#2519);
#2101=LINE('',#11231,#2520);
#2102=LINE('',#11236,#2521);
#2103=LINE('',#11244,#2522);
#2104=LINE('',#11248,#2523);
#2105=LINE('',#11252,#2524);
#2106=LINE('',#11259,#2525);
#2107=LINE('',#11263,#2526);
#2108=LINE('',#11267,#2527);
#2109=LINE('',#11272,#2528);
#2110=LINE('',#11274,#2529);
#2111=LINE('',#11276,#2530);
#2112=LINE('',#11277,#2531);
#2113=LINE('',#11280,#2532);
#2114=LINE('',#11282,#2533);
#2115=LINE('',#11283,#2534);
#2116=LINE('',#11286,#2535);
#2117=LINE('',#11288,#2536);
#2118=LINE('',#11289,#2537);
#2119=LINE('',#11292,#2538);
#2120=LINE('',#11294,#2539);
#2121=LINE('',#11295,#2540);
#2122=LINE('',#11298,#2541);
#2123=LINE('',#11300,#2542);
#2124=LINE('',#11301,#2543);
#2125=LINE('',#11303,#2544);
#2126=LINE('',#11304,#2545);
#2127=VECTOR('',#7267,0.21);
#2128=VECTOR('',#7274,0.21);
#2129=VECTOR('',#7281,0.21);
#2130=VECTOR('',#7288,0.21);
#2131=VECTOR('',#7293,1.);
#2132=VECTOR('',#7294,1.);
#2133=VECTOR('',#7295,1.);
#2134=VECTOR('',#7296,1.);
#2135=VECTOR('',#7299,1.);
#2136=VECTOR('',#7300,1.);
#2137=VECTOR('',#7301,1.);
#2138=VECTOR('',#7304,1.);
#2139=VECTOR('',#7305,1.);
#2140=VECTOR('',#7306,1.);
#2141=VECTOR('',#7309,1.);
#2142=VECTOR('',#7310,1.);
#2143=VECTOR('',#7321,0.165);
#2144=VECTOR('',#7330,0.5);
#2145=VECTOR('',#7341,0.5);
#2146=VECTOR('',#7352,0.275);
#2147=VECTOR('',#7357,0.275);
#2148=VECTOR('',#7360,1.);
#2149=VECTOR('',#7361,1.);
#2150=VECTOR('',#7362,1.);
#2151=VECTOR('',#7363,1.);
#2152=VECTOR('',#7366,1.);
#2153=VECTOR('',#7367,1.);
#2154=VECTOR('',#7368,1.);
#2155=VECTOR('',#7371,1.);
#2156=VECTOR('',#7372,1.);
#2157=VECTOR('',#7373,1.);
#2158=VECTOR('',#7376,1.);
#2159=VECTOR('',#7377,1.);
#2160=VECTOR('',#7388,0.165);
#2161=VECTOR('',#7397,0.5);
#2162=VECTOR('',#7408,0.5);
#2163=VECTOR('',#7419,0.275);
#2164=VECTOR('',#7424,0.275);
#2165=VECTOR('',#7427,1.);
#2166=VECTOR('',#7428,1.);
#2167=VECTOR('',#7429,1.);
#2168=VECTOR('',#7430,1.);
#2169=VECTOR('',#7433,1.);
#2170=VECTOR('',#7434,1.);
#2171=VECTOR('',#7435,1.);
#2172=VECTOR('',#7438,1.);
#2173=VECTOR('',#7439,1.);
#2174=VECTOR('',#7440,1.);
#2175=VECTOR('',#7443,1.);
#2176=VECTOR('',#7444,1.);
#2177=VECTOR('',#7453,1.);
#2178=VECTOR('',#7458,1.);
#2179=VECTOR('',#7463,1.);
#2180=VECTOR('',#7468,1.);
#2181=VECTOR('',#7469,1.);
#2182=VECTOR('',#7474,0.4);
#2183=VECTOR('',#7495,1.);
#2184=VECTOR('',#7498,1.);
#2185=VECTOR('',#7511,0.4);
#2186=VECTOR('',#7524,0.685);
#2187=VECTOR('',#7531,0.15);
#2188=VECTOR('',#7538,0.25);
#2189=VECTOR('',#7547,0.2);
#2190=VECTOR('',#7552,0.515);
#2191=VECTOR('',#7559,0.15);
#2192=VECTOR('',#7566,0.25);
#2193=VECTOR('',#7575,0.2);
#2194=VECTOR('',#7580,0.515);
#2195=VECTOR('',#7587,0.15);
#2196=VECTOR('',#7594,0.25);
#2197=VECTOR('',#7603,0.2);
#2198=VECTOR('',#7608,0.515);
#2199=VECTOR('',#7615,0.15);
#2200=VECTOR('',#7622,0.25);
#2201=VECTOR('',#7631,0.2);
#2202=VECTOR('',#7636,0.515);
#2203=VECTOR('',#7645,0.3);
#2204=VECTOR('',#7646,0.3);
#2205=VECTOR('',#7647,0.3);
#2206=VECTOR('',#7648,0.3);
#2207=VECTOR('',#7649,0.3);
#2208=VECTOR('',#7650,0.3);
#2209=VECTOR('',#7657,0.4);
#2210=VECTOR('',#7668,0.4);
#2211=VECTOR('',#7679,0.4);
#2212=VECTOR('',#7690,0.4);
#2213=VECTOR('',#7701,0.225);
#2214=VECTOR('',#7706,0.225);
#2215=VECTOR('',#7711,0.225);
#2216=VECTOR('',#7716,0.225);
#2217=VECTOR('',#7719,1.);
#2218=VECTOR('',#7720,1.);
#2219=VECTOR('',#7721,1.);
#2220=VECTOR('',#7722,1.);
#2221=VECTOR('',#7725,1.);
#2222=VECTOR('',#7726,1.);
#2223=VECTOR('',#7727,1.);
#2224=VECTOR('',#7730,1.);
#2225=VECTOR('',#7731,1.);
#2226=VECTOR('',#7732,1.);
#2227=VECTOR('',#7735,1.);
#2228=VECTOR('',#7736,1.);
#2229=VECTOR('',#7747,0.2);
#2230=VECTOR('',#7754,0.3);
#2231=VECTOR('',#7773,0.6);
#2232=VECTOR('',#7784,0.3);
#2233=VECTOR('',#7787,0.1);
#2234=VECTOR('',#7798,0.3);
#2235=VECTOR('',#7805,0.5);
#2236=VECTOR('',#7818,0.2);
#2237=VECTOR('',#7825,0.3);
#2238=VECTOR('',#7844,0.6);
#2239=VECTOR('',#7855,0.3);
#2240=VECTOR('',#7858,0.1);
#2241=VECTOR('',#7869,0.3);
#2242=VECTOR('',#7876,0.5);
#2243=VECTOR('',#7889,0.2);
#2244=VECTOR('',#7896,0.3);
#2245=VECTOR('',#7915,0.6);
#2246=VECTOR('',#7926,0.3);
#2247=VECTOR('',#7929,0.1);
#2248=VECTOR('',#7940,0.3);
#2249=VECTOR('',#7947,0.5);
#2250=VECTOR('',#7960,0.2);
#2251=VECTOR('',#7967,0.3);
#2252=VECTOR('',#7986,0.6);
#2253=VECTOR('',#7997,0.3);
#2254=VECTOR('',#8000,0.1);
#2255=VECTOR('',#8011,0.3);
#2256=VECTOR('',#8018,0.5);
#2257=VECTOR('',#8031,0.3);
#2258=VECTOR('',#8044,0.3);
#2259=VECTOR('',#8057,0.165);
#2260=VECTOR('',#8066,0.165);
#2261=VECTOR('',#8075,0.165);
#2262=VECTOR('',#8084,0.165);
#2263=VECTOR('',#8093,0.08);
#2264=VECTOR('',#8098,0.08);
#2265=VECTOR('',#8103,0.08);
#2266=VECTOR('',#8108,0.08);
#2267=VECTOR('',#8111,1.);
#2268=VECTOR('',#8112,1.);
#2269=VECTOR('',#8113,1.);
#2270=VECTOR('',#8114,1.);
#2271=VECTOR('',#8119,1.);
#2272=VECTOR('',#8120,1.);
#2273=VECTOR('',#8125,1.);
#2274=VECTOR('',#8126,1.);
#2275=VECTOR('',#8131,1.);
#2276=VECTOR('',#8134,1.);
#2277=VECTOR('',#8135,1.);
#2278=VECTOR('',#8140,1.);
#2279=VECTOR('',#8143,1.);
#2280=VECTOR('',#8144,1.);
#2281=VECTOR('',#8145,1.);
#2282=VECTOR('',#8146,1.);
#2283=VECTOR('',#8147,1.);
#2284=VECTOR('',#8150,1.);
#2285=VECTOR('',#8151,1.);
#2286=VECTOR('',#8152,1.);
#2287=VECTOR('',#8157,1.);
#2288=VECTOR('',#8158,1.);
#2289=VECTOR('',#8161,1.);
#2290=VECTOR('',#8162,1.);
#2291=VECTOR('',#8163,1.);
#2292=VECTOR('',#8168,1.);
#2293=VECTOR('',#8171,1.);
#2294=VECTOR('',#8172,1.);
#2295=VECTOR('',#8177,0.685);
#2296=VECTOR('',#8184,2.5);
#2297=VECTOR('',#8185,2.5);
#2298=VECTOR('',#8194,3.);
#2299=VECTOR('',#8207,0.12);
#2300=VECTOR('',#8214,0.12);
#2301=VECTOR('',#8221,0.12);
#2302=VECTOR('',#8228,0.12);
#2303=VECTOR('',#8233,1.);
#2304=VECTOR('',#8234,1.);
#2305=VECTOR('',#8235,1.);
#2306=VECTOR('',#8236,1.);
#2307=VECTOR('',#8239,1.);
#2308=VECTOR('',#8240,1.);
#2309=VECTOR('',#8241,1.);
#2310=VECTOR('',#8244,1.);
#2311=VECTOR('',#8245,1.);
#2312=VECTOR('',#8246,1.);
#2313=VECTOR('',#8249,1.);
#2314=VECTOR('',#8250,1.);
#2315=VECTOR('',#8253,1.);
#2316=VECTOR('',#8254,1.);
#2317=VECTOR('',#8255,1.);
#2318=VECTOR('',#8256,1.);
#2319=VECTOR('',#8259,1.);
#2320=VECTOR('',#8260,1.);
#2321=VECTOR('',#8261,1.);
#2322=VECTOR('',#8264,1.);
#2323=VECTOR('',#8265,1.);
#2324=VECTOR('',#8266,1.);
#2325=VECTOR('',#8269,1.);
#2326=VECTOR('',#8270,1.);
#2327=VECTOR('',#8281,0.12);
#2328=VECTOR('',#8288,0.12);
#2329=VECTOR('',#8295,0.12);
#2330=VECTOR('',#8302,0.12);
#2331=VECTOR('',#8307,1.);
#2332=VECTOR('',#8308,1.);
#2333=VECTOR('',#8309,1.);
#2334=VECTOR('',#8310,1.);
#2335=VECTOR('',#8313,1.);
#2336=VECTOR('',#8314,1.);
#2337=VECTOR('',#8315,1.);
#2338=VECTOR('',#8318,1.);
#2339=VECTOR('',#8319,1.);
#2340=VECTOR('',#8320,1.);
#2341=VECTOR('',#8323,1.);
#2342=VECTOR('',#8324,1.);
#2343=VECTOR('',#8335,0.12);
#2344=VECTOR('',#8342,0.12);
#2345=VECTOR('',#8349,0.12);
#2346=VECTOR('',#8356,0.12);
#2347=VECTOR('',#8361,1.);
#2348=VECTOR('',#8362,1.);
#2349=VECTOR('',#8363,1.);
#2350=VECTOR('',#8364,1.);
#2351=VECTOR('',#8367,1.);
#2352=VECTOR('',#8368,1.);
#2353=VECTOR('',#8369,1.);
#2354=VECTOR('',#8372,1.);
#2355=VECTOR('',#8373,1.);
#2356=VECTOR('',#8374,1.);
#2357=VECTOR('',#8377,1.);
#2358=VECTOR('',#8378,1.);
#2359=VECTOR('',#8381,1.);
#2360=VECTOR('',#8382,1.);
#2361=VECTOR('',#8383,1.);
#2362=VECTOR('',#8384,1.);
#2363=VECTOR('',#8387,1.);
#2364=VECTOR('',#8388,1.);
#2365=VECTOR('',#8389,1.);
#2366=VECTOR('',#8392,1.);
#2367=VECTOR('',#8393,1.);
#2368=VECTOR('',#8394,1.);
#2369=VECTOR('',#8397,1.);
#2370=VECTOR('',#8398,1.);
#2371=VECTOR('',#8407,1.);
#2372=VECTOR('',#8408,1.);
#2373=VECTOR('',#8409,1.);
#2374=VECTOR('',#8410,1.);
#2375=VECTOR('',#8413,1.);
#2376=VECTOR('',#8414,1.);
#2377=VECTOR('',#8415,1.);
#2378=VECTOR('',#8416,1.);
#2379=VECTOR('',#8441,0.175);
#2380=VECTOR('',#8446,0.1);
#2381=VECTOR('',#8453,1.);
#2382=VECTOR('',#8454,1.);
#2383=VECTOR('',#8455,1.);
#2384=VECTOR('',#8456,1.);
#2385=VECTOR('',#8459,1.);
#2386=VECTOR('',#8460,1.);
#2387=VECTOR('',#8461,1.);
#2388=VECTOR('',#8462,1.);
#2389=VECTOR('',#8487,0.175);
#2390=VECTOR('',#8492,0.1);
#2391=VECTOR('',#8499,1.);
#2392=VECTOR('',#8500,1.);
#2393=VECTOR('',#8501,1.);
#2394=VECTOR('',#8502,1.);
#2395=VECTOR('',#8505,1.);
#2396=VECTOR('',#8506,1.);
#2397=VECTOR('',#8507,1.);
#2398=VECTOR('',#8508,1.);
#2399=VECTOR('',#8533,0.175);
#2400=VECTOR('',#8538,0.1);
#2401=VECTOR('',#8545,1.);
#2402=VECTOR('',#8546,1.);
#2403=VECTOR('',#8547,1.);
#2404=VECTOR('',#8548,1.);
#2405=VECTOR('',#8551,1.);
#2406=VECTOR('',#8552,1.);
#2407=VECTOR('',#8553,1.);
#2408=VECTOR('',#8554,1.);
#2409=VECTOR('',#8579,0.175);
#2410=VECTOR('',#8584,0.1);
#2411=VECTOR('',#8593,0.225);
#2412=VECTOR('',#8600,0.225);
#2413=VECTOR('',#8607,0.225);
#2414=VECTOR('',#8614,0.225);
#2415=VECTOR('',#8621,2.5);
#2416=VECTOR('',#8628,3.);
#2417=VECTOR('',#8641,0.6);
#2418=VECTOR('',#8648,0.225);
#2419=VECTOR('',#8655,0.225);
#2420=VECTOR('',#8662,0.225);
#2421=VECTOR('',#8669,0.225);
#2422=VECTOR('',#8676,3.);
#2423=VECTOR('',#8689,0.075);
#2424=VECTOR('',#8702,1.);
#2425=VECTOR('',#8707,0.6);
#2426=VECTOR('',#8716,1.);
#2427=VECTOR('',#8717,1.);
#2428=VECTOR('',#8718,1.);
#2429=VECTOR('',#8719,1.);
#2430=VECTOR('',#8722,1.);
#2431=VECTOR('',#8723,1.);
#2432=VECTOR('',#8724,1.);
#2433=VECTOR('',#8727,1.);
#2434=VECTOR('',#8728,1.);
#2435=VECTOR('',#8729,1.);
#2436=VECTOR('',#8732,1.);
#2437=VECTOR('',#8733,1.);
#2438=VECTOR('',#8742,1.);
#2439=VECTOR('',#8743,1.);
#2440=VECTOR('',#8744,1.);
#2441=VECTOR('',#8745,1.);
#2442=VECTOR('',#8748,1.);
#2443=VECTOR('',#8749,1.);
#2444=VECTOR('',#8750,1.);
#2445=VECTOR('',#8753,1.);
#2446=VECTOR('',#8754,1.);
#2447=VECTOR('',#8755,1.);
#2448=VECTOR('',#8758,1.);
#2449=VECTOR('',#8759,1.);
#2450=VECTOR('',#8768,1.);
#2451=VECTOR('',#8769,1.);
#2452=VECTOR('',#8770,1.);
#2453=VECTOR('',#8771,1.);
#2454=VECTOR('',#8774,1.);
#2455=VECTOR('',#8775,1.);
#2456=VECTOR('',#8776,1.);
#2457=VECTOR('',#8779,1.);
#2458=VECTOR('',#8780,1.);
#2459=VECTOR('',#8781,1.);
#2460=VECTOR('',#8784,1.);
#2461=VECTOR('',#8785,1.);
#2462=VECTOR('',#8786,1.);
#2463=VECTOR('',#8789,1.);
#2464=VECTOR('',#8790,1.);
#2465=VECTOR('',#8791,1.);
#2466=VECTOR('',#8794,1.);
#2467=VECTOR('',#8795,1.);
#2468=VECTOR('',#8812,0.4);
#2469=VECTOR('',#8817,0.425);
#2470=VECTOR('',#8822,0.41);
#2471=VECTOR('',#8831,0.26);
#2472=VECTOR('',#8834,0.25);
#2473=VECTOR('',#8843,0.43);
#2474=VECTOR('',#8852,1.);
#2475=VECTOR('',#8853,1.);
#2476=VECTOR('',#8854,1.);
#2477=VECTOR('',#8855,1.);
#2478=VECTOR('',#8856,1.);
#2479=VECTOR('',#8857,1.);
#2480=VECTOR('',#8862,1.);
#2481=VECTOR('',#8863,1.);
#2482=VECTOR('',#8864,1.);
#2483=VECTOR('',#8865,1.);
#2484=VECTOR('',#8866,1.);
#2485=VECTOR('',#8867,1.);
#2486=VECTOR('',#8872,1.);
#2487=VECTOR('',#8873,1.);
#2488=VECTOR('',#8876,1.);
#2489=VECTOR('',#8879,1.);
#2490=VECTOR('',#8882,1.);
#2491=VECTOR('',#8885,1.);
#2492=VECTOR('',#8894,0.46);
#2493=VECTOR('',#8903,0.525);
#2494=VECTOR('',#8908,0.515);
#2495=VECTOR('',#8915,0.2);
#2496=VECTOR('',#8928,0.475);
#2497=VECTOR('',#8937,0.355);
#2498=VECTOR('',#8944,0.31);
#2499=VECTOR('',#8953,1.);
#2500=VECTOR('',#8954,1.);
#2501=VECTOR('',#8955,1.);
#2502=VECTOR('',#8956,1.);
#2503=VECTOR('',#8957,1.);
#2504=VECTOR('',#8958,1.);
#2505=VECTOR('',#8963,1.);
#2506=VECTOR('',#8964,1.);
#2507=VECTOR('',#8965,1.);
#2508=VECTOR('',#8966,1.);
#2509=VECTOR('',#8967,1.);
#2510=VECTOR('',#8968,1.);
#2511=VECTOR('',#8973,1.);
#2512=VECTOR('',#8974,1.);
#2513=VECTOR('',#8977,1.);
#2514=VECTOR('',#8980,1.);
#2515=VECTOR('',#8983,1.);
#2516=VECTOR('',#8986,1.);
#2517=VECTOR('',#8991,0.685);
#2518=VECTOR('',#9002,0.645);
#2519=VECTOR('',#9007,0.685);
#2520=VECTOR('',#9012,0.645);
#2521=VECTOR('',#9019,0.46);
#2522=VECTOR('',#9030,0.325);
#2523=VECTOR('',#9035,0.35);
#2524=VECTOR('',#9040,0.335);
#2525=VECTOR('',#9049,0.21);
#2526=VECTOR('',#9054,0.2);
#2527=VECTOR('',#9059,0.18);
#2528=VECTOR('',#9064,1.);
#2529=VECTOR('',#9065,1.);
#2530=VECTOR('',#9066,1.);
#2531=VECTOR('',#9067,1.);
#2532=VECTOR('',#9070,1.);
#2533=VECTOR('',#9071,1.);
#2534=VECTOR('',#9072,1.);
#2535=VECTOR('',#9075,1.);
#2536=VECTOR('',#9076,1.);
#2537=VECTOR('',#9077,1.);
#2538=VECTOR('',#9080,1.);
#2539=VECTOR('',#9081,1.);
#2540=VECTOR('',#9082,1.);
#2541=VECTOR('',#9085,1.);
#2542=VECTOR('',#9086,1.);
#2543=VECTOR('',#9087,1.);
#2544=VECTOR('',#9090,1.);
#2545=VECTOR('',#9091,1.);
#2546=CIRCLE('',#6505,0.21);
#2547=CIRCLE('',#6506,0.21);
#2548=CIRCLE('',#6508,0.21);
#2549=CIRCLE('',#6509,0.21);
#2550=CIRCLE('',#6511,0.21);
#2551=CIRCLE('',#6512,0.21);
#2552=CIRCLE('',#6514,0.21);
#2553=CIRCLE('',#6515,0.21);
#2554=CIRCLE('',#6524,0.165);
#2555=CIRCLE('',#6525,0.165);
#2556=CIRCLE('',#6528,0.5);
#2557=CIRCLE('',#6529,0.5);
#2558=CIRCLE('',#6531,0.275);
#2559=CIRCLE('',#6533,0.5);
#2560=CIRCLE('',#6534,0.5);
#2561=CIRCLE('',#6536,0.275);
#2562=CIRCLE('',#6538,0.275);
#2563=CIRCLE('',#6540,0.275);
#2564=CIRCLE('',#6549,0.165);
#2565=CIRCLE('',#6550,0.165);
#2566=CIRCLE('',#6553,0.5);
#2567=CIRCLE('',#6554,0.5);
#2568=CIRCLE('',#6556,0.275);
#2569=CIRCLE('',#6558,0.5);
#2570=CIRCLE('',#6559,0.5);
#2571=CIRCLE('',#6561,0.275);
#2572=CIRCLE('',#6563,0.275);
#2573=CIRCLE('',#6565,0.275);
#2574=CIRCLE('',#6574,0.4);
#2575=CIRCLE('',#6576,0.4);
#2576=CIRCLE('',#6578,0.4);
#2577=CIRCLE('',#6582,0.4);
#2578=CIRCLE('',#6589,0.4);
#2579=CIRCLE('',#6594,0.4);
#2580=CIRCLE('',#6596,0.4);
#2581=CIRCLE('',#6599,0.4);
#2582=CIRCLE('',#6601,0.4);
#2583=CIRCLE('',#6604,0.685);
#2584=CIRCLE('',#6605,0.685);
#2585=CIRCLE('',#6608,0.15);
#2586=CIRCLE('',#6610,0.25);
#2587=CIRCLE('',#6611,0.25);
#2588=CIRCLE('',#6614,0.2);
#2589=CIRCLE('',#6616,0.515);
#2590=CIRCLE('',#6617,0.515);
#2591=CIRCLE('',#6620,0.15);
#2592=CIRCLE('',#6622,0.25);
#2593=CIRCLE('',#6623,0.25);
#2594=CIRCLE('',#6626,0.2);
#2595=CIRCLE('',#6628,0.515);
#2596=CIRCLE('',#6629,0.515);
#2597=CIRCLE('',#6632,0.15);
#2598=CIRCLE('',#6634,0.25);
#2599=CIRCLE('',#6635,0.25);
#2600=CIRCLE('',#6638,0.2);
#2601=CIRCLE('',#6640,0.515);
#2602=CIRCLE('',#6641,0.515);
#2603=CIRCLE('',#6644,0.15);
#2604=CIRCLE('',#6646,0.25);
#2605=CIRCLE('',#6647,0.25);
#2606=CIRCLE('',#6650,0.2);
#2607=CIRCLE('',#6652,0.515);
#2608=CIRCLE('',#6653,0.515);
#2609=CIRCLE('',#6656,0.3);
#2610=CIRCLE('',#6657,0.3);
#2611=CIRCLE('',#6659,0.4);
#2612=CIRCLE('',#6660,0.4);
#2613=CIRCLE('',#6662,0.225);
#2614=CIRCLE('',#6664,0.4);
#2615=CIRCLE('',#6665,0.4);
#2616=CIRCLE('',#6667,0.225);
#2617=CIRCLE('',#6669,0.4);
#2618=CIRCLE('',#6670,0.4);
#2619=CIRCLE('',#6672,0.225);
#2620=CIRCLE('',#6674,0.4);
#2621=CIRCLE('',#6675,0.4);
#2622=CIRCLE('',#6677,0.225);
#2623=CIRCLE('',#6679,0.225);
#2624=CIRCLE('',#6681,0.225);
#2625=CIRCLE('',#6683,0.225);
#2626=CIRCLE('',#6685,0.225);
#2627=CIRCLE('',#6694,0.2);
#2628=CIRCLE('',#6695,0.2);
#2629=CIRCLE('',#6697,0.3);
#2630=CIRCLE('',#6698,0.3);
#2631=CIRCLE('',#6703,0.6);
#2632=CIRCLE('',#6704,0.3);
#2633=CIRCLE('',#6706,0.6);
#2634=CIRCLE('',#6709,0.3);
#2635=CIRCLE('',#6710,0.1);
#2636=CIRCLE('',#6713,0.1);
#2637=CIRCLE('',#6717,0.3);
#2638=CIRCLE('',#6718,0.3);
#2639=CIRCLE('',#6720,0.5);
#2640=CIRCLE('',#6721,0.5);
#2641=CIRCLE('',#6726,0.2);
#2642=CIRCLE('',#6727,0.2);
#2643=CIRCLE('',#6729,0.3);
#2644=CIRCLE('',#6730,0.3);
#2645=CIRCLE('',#6735,0.6);
#2646=CIRCLE('',#6736,0.3);
#2647=CIRCLE('',#6738,0.6);
#2648=CIRCLE('',#6741,0.3);
#2649=CIRCLE('',#6742,0.1);
#2650=CIRCLE('',#6745,0.1);
#2651=CIRCLE('',#6749,0.3);
#2652=CIRCLE('',#6750,0.3);
#2653=CIRCLE('',#6752,0.5);
#2654=CIRCLE('',#6753,0.5);
#2655=CIRCLE('',#6758,0.2);
#2656=CIRCLE('',#6759,0.2);
#2657=CIRCLE('',#6761,0.3);
#2658=CIRCLE('',#6762,0.3);
#2659=CIRCLE('',#6767,0.6);
#2660=CIRCLE('',#6768,0.3);
#2661=CIRCLE('',#6770,0.6);
#2662=CIRCLE('',#6773,0.3);
#2663=CIRCLE('',#6774,0.1);
#2664=CIRCLE('',#6777,0.1);
#2665=CIRCLE('',#6781,0.3);
#2666=CIRCLE('',#6782,0.3);
#2667=CIRCLE('',#6784,0.5);
#2668=CIRCLE('',#6785,0.5);
#2669=CIRCLE('',#6790,0.2);
#2670=CIRCLE('',#6791,0.2);
#2671=CIRCLE('',#6793,0.3);
#2672=CIRCLE('',#6794,0.3);
#2673=CIRCLE('',#6799,0.6);
#2674=CIRCLE('',#6800,0.3);
#2675=CIRCLE('',#6802,0.6);
#2676=CIRCLE('',#6805,0.3);
#2677=CIRCLE('',#6806,0.1);
#2678=CIRCLE('',#6809,0.1);
#2679=CIRCLE('',#6813,0.3);
#2680=CIRCLE('',#6814,0.3);
#2681=CIRCLE('',#6816,0.5);
#2682=CIRCLE('',#6817,0.5);
#2683=CIRCLE('',#6822,0.3);
#2684=CIRCLE('',#6823,0.3);
#2685=CIRCLE('',#6828,0.3);
#2686=CIRCLE('',#6829,0.3);
#2687=CIRCLE('',#6834,0.165);
#2688=CIRCLE('',#6835,0.165);
#2689=CIRCLE('',#6838,0.165);
#2690=CIRCLE('',#6839,0.165);
#2691=CIRCLE('',#6842,0.165);
#2692=CIRCLE('',#6843,0.165);
#2693=CIRCLE('',#6846,0.165);
#2694=CIRCLE('',#6847,0.165);
#2695=CIRCLE('',#6850,0.08);
#2696=CIRCLE('',#6852,0.08);
#2697=CIRCLE('',#6854,0.08);
#2698=CIRCLE('',#6856,0.08);
#2699=CIRCLE('',#6859,2.5);
#2700=CIRCLE('',#6861,2.5);
#2701=CIRCLE('',#6863,2.5);
#2702=CIRCLE('',#6866,2.5);
#2703=CIRCLE('',#6870,3.);
#2704=CIRCLE('',#6873,3.);
#2705=CIRCLE('',#6876,0.685);
#2706=CIRCLE('',#6877,0.685);
#2707=CIRCLE('',#6879,2.5);
#2708=CIRCLE('',#6880,2.5);
#2709=CIRCLE('',#6883,3.);
#2710=CIRCLE('',#6884,3.);
#2711=CIRCLE('',#6889,0.12);
#2712=CIRCLE('',#6890,0.12);
#2713=CIRCLE('',#6892,0.12);
#2714=CIRCLE('',#6893,0.12);
#2715=CIRCLE('',#6895,0.12);
#2716=CIRCLE('',#6896,0.12);
#2717=CIRCLE('',#6898,0.12);
#2718=CIRCLE('',#6899,0.12);
#2719=CIRCLE('',#6912,0.12);
#2720=CIRCLE('',#6913,0.12);
#2721=CIRCLE('',#6915,0.12);
#2722=CIRCLE('',#6916,0.12);
#2723=CIRCLE('',#6918,0.12);
#2724=CIRCLE('',#6919,0.12);
#2725=CIRCLE('',#6921,0.12);
#2726=CIRCLE('',#6922,0.12);
#2727=CIRCLE('',#6931,0.12);
#2728=CIRCLE('',#6932,0.12);
#2729=CIRCLE('',#6934,0.12);
#2730=CIRCLE('',#6935,0.12);
#2731=CIRCLE('',#6937,0.12);
#2732=CIRCLE('',#6938,0.12);
#2733=CIRCLE('',#6940,0.12);
#2734=CIRCLE('',#6941,0.12);
#2735=CIRCLE('',#6956,0.175);
#2736=CIRCLE('',#6957,0.175);
#2737=CIRCLE('',#6959,0.175);
#2738=CIRCLE('',#6961,0.175);
#2739=CIRCLE('',#6962,0.175);
#2740=CIRCLE('',#6964,0.175);
#2741=CIRCLE('',#6965,0.1);
#2742=CIRCLE('',#6968,0.1);
#2743=CIRCLE('',#6974,0.175);
#2744=CIRCLE('',#6975,0.175);
#2745=CIRCLE('',#6977,0.175);
#2746=CIRCLE('',#6979,0.175);
#2747=CIRCLE('',#6980,0.175);
#2748=CIRCLE('',#6982,0.175);
#2749=CIRCLE('',#6983,0.1);
#2750=CIRCLE('',#6986,0.1);
#2751=CIRCLE('',#6992,0.175);
#2752=CIRCLE('',#6993,0.175);
#2753=CIRCLE('',#6995,0.175);
#2754=CIRCLE('',#6997,0.175);
#2755=CIRCLE('',#6998,0.175);
#2756=CIRCLE('',#7000,0.175);
#2757=CIRCLE('',#7001,0.1);
#2758=CIRCLE('',#7004,0.1);
#2759=CIRCLE('',#7010,0.175);
#2760=CIRCLE('',#7011,0.175);
#2761=CIRCLE('',#7013,0.175);
#2762=CIRCLE('',#7015,0.175);
#2763=CIRCLE('',#7016,0.175);
#2764=CIRCLE('',#7018,0.175);
#2765=CIRCLE('',#7019,0.1);
#2766=CIRCLE('',#7022,0.1);
#2767=CIRCLE('',#7026,0.225);
#2768=CIRCLE('',#7027,0.225);
#2769=CIRCLE('',#7029,0.225);
#2770=CIRCLE('',#7030,0.225);
#2771=CIRCLE('',#7032,0.225);
#2772=CIRCLE('',#7033,0.225);
#2773=CIRCLE('',#7035,0.225);
#2774=CIRCLE('',#7036,0.225);
#2775=CIRCLE('',#7038,2.5);
#2776=CIRCLE('',#7039,2.5);
#2777=CIRCLE('',#7041,3.);
#2778=CIRCLE('',#7042,3.);
#2779=CIRCLE('',#7047,0.6);
#2780=CIRCLE('',#7048,0.6);
#2781=CIRCLE('',#7050,0.225);
#2782=CIRCLE('',#7051,0.225);
#2783=CIRCLE('',#7053,0.225);
#2784=CIRCLE('',#7054,0.225);
#2785=CIRCLE('',#7056,0.225);
#2786=CIRCLE('',#7057,0.225);
#2787=CIRCLE('',#7059,0.225);
#2788=CIRCLE('',#7060,0.225);
#2789=CIRCLE('',#7062,3.);
#2790=CIRCLE('',#7063,3.);
#2791=CIRCLE('',#7068,0.075);
#2792=CIRCLE('',#7069,0.075);
#2793=CIRCLE('',#7071,1.);
#2794=CIRCLE('',#7072,0.6);
#2795=CIRCLE('',#7074,1.);
#2796=CIRCLE('',#7077,0.6);
#2797=CIRCLE('',#7103,0.24505);
#2798=CIRCLE('',#7105,0.375);
#2799=CIRCLE('',#7107,0.425);
#2800=CIRCLE('',#7109,0.425);
#2801=CIRCLE('',#7111,0.395);
#2802=CIRCLE('',#7113,0.27);
#2803=CIRCLE('',#7115,0.24505);
#2804=CIRCLE('',#7120,0.43);
#2805=CIRCLE('',#7121,0.43);
#2806=CIRCLE('',#7123,0.2);
#2807=CIRCLE('',#7125,0.525);
#2808=CIRCLE('',#7127,0.515);
#2809=CIRCLE('',#7135,0.46);
#2810=CIRCLE('',#7137,0.46);
#2811=CIRCLE('',#7139,0.525);
#2812=CIRCLE('',#7142,0.515);
#2813=CIRCLE('',#7144,0.2);
#2814=CIRCLE('',#7148,0.475);
#2815=CIRCLE('',#7149,0.31);
#2816=CIRCLE('',#7151,0.475);
#2817=CIRCLE('',#7153,0.355);
#2818=CIRCLE('',#7155,0.355);
#2819=CIRCLE('',#7157,0.31);
#2820=CIRCLE('',#7163,0.685);
#2821=CIRCLE('',#7165,0.685);
#2822=CIRCLE('',#7173,0.685);
#2823=CIRCLE('',#7175,0.605);
#2824=CIRCLE('',#7176,0.46);
#2825=CIRCLE('',#7179,0.685);
#2826=CIRCLE('',#7181,0.605);
#2827=CIRCLE('',#7183,0.46);
#2828=CIRCLE('',#7187,0.3);
#2829=CIRCLE('',#7189,0.35);
#2830=CIRCLE('',#7191,0.35);
#2831=CIRCLE('',#7193,0.32);
#2832=CIRCLE('',#7195,0.22);
#2833=CIRCLE('',#7197,0.1954);
#2834=CIRCLE('',#7199,0.1954);
#2835=CIRCLE('',#7201,0.16);
#2836=VERTEX_POINT('',#9195);
#2837=VERTEX_POINT('',#9197);
#2838=VERTEX_POINT('',#9201);
#2839=VERTEX_POINT('',#9203);
#2840=VERTEX_POINT('',#9207);
#2841=VERTEX_POINT('',#9209);
#2842=VERTEX_POINT('',#9213);
#2843=VERTEX_POINT('',#9215);
#2844=VERTEX_POINT('',#9219);
#2845=VERTEX_POINT('',#9220);
#2846=VERTEX_POINT('',#9222);
#2847=VERTEX_POINT('',#9224);
#2848=VERTEX_POINT('',#9228);
#2849=VERTEX_POINT('',#9230);
#2850=VERTEX_POINT('',#9234);
#2851=VERTEX_POINT('',#9236);
#2852=VERTEX_POINT('',#9246);
#2853=VERTEX_POINT('',#9248);
#2854=VERTEX_POINT('',#9253);
#2855=VERTEX_POINT('',#9255);
#2856=VERTEX_POINT('',#9259);
#2857=VERTEX_POINT('',#9262);
#2858=VERTEX_POINT('',#9264);
#2859=VERTEX_POINT('',#9268);
#2860=VERTEX_POINT('',#9271);
#2861=VERTEX_POINT('',#9275);
#2862=VERTEX_POINT('',#9279);
#2863=VERTEX_POINT('',#9280);
#2864=VERTEX_POINT('',#9282);
#2865=VERTEX_POINT('',#9284);
#2866=VERTEX_POINT('',#9288);
#2867=VERTEX_POINT('',#9290);
#2868=VERTEX_POINT('',#9294);
#2869=VERTEX_POINT('',#9296);
#2870=VERTEX_POINT('',#9306);
#2871=VERTEX_POINT('',#9308);
#2872=VERTEX_POINT('',#9313);
#2873=VERTEX_POINT('',#9315);
#2874=VERTEX_POINT('',#9319);
#2875=VERTEX_POINT('',#9322);
#2876=VERTEX_POINT('',#9324);
#2877=VERTEX_POINT('',#9328);
#2878=VERTEX_POINT('',#9331);
#2879=VERTEX_POINT('',#9335);
#2880=VERTEX_POINT('',#9339);
#2881=VERTEX_POINT('',#9340);
#2882=VERTEX_POINT('',#9342);
#2883=VERTEX_POINT('',#9344);
#2884=VERTEX_POINT('',#9348);
#2885=VERTEX_POINT('',#9350);
#2886=VERTEX_POINT('',#9354);
#2887=VERTEX_POINT('',#9356);
#2888=VERTEX_POINT('',#9366);
#2889=VERTEX_POINT('',#9367);
#2890=VERTEX_POINT('',#9371);
#2891=VERTEX_POINT('',#9375);
#2892=VERTEX_POINT('',#9376);
#2893=VERTEX_POINT('',#9380);
#2894=VERTEX_POINT('',#9382);
#2895=VERTEX_POINT('',#9384);
#2896=VERTEX_POINT('',#9386);
#2897=VERTEX_POINT('',#9388);
#2898=VERTEX_POINT('',#9390);
#2899=VERTEX_POINT('',#9409);
#2900=VERTEX_POINT('',#9416);
#2901=VERTEX_POINT('',#9444);
#2902=VERTEX_POINT('',#9468);
#2903=VERTEX_POINT('',#9482);
#2904=VERTEX_POINT('',#9489);
#2905=VERTEX_POINT('',#9491);
#2906=VERTEX_POINT('',#9496);
#2907=VERTEX_POINT('',#9497);
#2908=VERTEX_POINT('',#9508);
#2909=VERTEX_POINT('',#9519);
#2910=VERTEX_POINT('',#9541);
#2911=VERTEX_POINT('',#9543);
#2912=VERTEX_POINT('',#9548);
#2913=VERTEX_POINT('',#9550);
#2914=VERTEX_POINT('',#9552);
#2915=VERTEX_POINT('',#9590);
#2916=VERTEX_POINT('',#9592);
#2917=VERTEX_POINT('',#9597);
#2918=VERTEX_POINT('',#9598);
#2919=VERTEX_POINT('',#9609);
#2920=VERTEX_POINT('',#9620);
#2921=VERTEX_POINT('',#9642);
#2922=VERTEX_POINT('',#9644);
#2923=VERTEX_POINT('',#9649);
#2924=VERTEX_POINT('',#9651);
#2925=VERTEX_POINT('',#9653);
#2926=VERTEX_POINT('',#9691);
#2927=VERTEX_POINT('',#9693);
#2928=VERTEX_POINT('',#9698);
#2929=VERTEX_POINT('',#9699);
#2930=VERTEX_POINT('',#9710);
#2931=VERTEX_POINT('',#9721);
#2932=VERTEX_POINT('',#9743);
#2933=VERTEX_POINT('',#9745);
#2934=VERTEX_POINT('',#9750);
#2935=VERTEX_POINT('',#9752);
#2936=VERTEX_POINT('',#9754);
#2937=VERTEX_POINT('',#9792);
#2938=VERTEX_POINT('',#9794);
#2939=VERTEX_POINT('',#9799);
#2940=VERTEX_POINT('',#9800);
#2941=VERTEX_POINT('',#9811);
#2942=VERTEX_POINT('',#9822);
#2943=VERTEX_POINT('',#9844);
#2944=VERTEX_POINT('',#9846);
#2945=VERTEX_POINT('',#9851);
#2946=VERTEX_POINT('',#9853);
#2947=VERTEX_POINT('',#9855);
#2948=VERTEX_POINT('',#9893);
#2949=VERTEX_POINT('',#9895);
#2950=VERTEX_POINT('',#9900);
#2951=VERTEX_POINT('',#9907);
#2952=VERTEX_POINT('',#9911);
#2953=VERTEX_POINT('',#9913);
#2954=VERTEX_POINT('',#9917);
#2955=VERTEX_POINT('',#9920);
#2956=VERTEX_POINT('',#9922);
#2957=VERTEX_POINT('',#9926);
#2958=VERTEX_POINT('',#9929);
#2959=VERTEX_POINT('',#9931);
#2960=VERTEX_POINT('',#9935);
#2961=VERTEX_POINT('',#9938);
#2962=VERTEX_POINT('',#9940);
#2963=VERTEX_POINT('',#9944);
#2964=VERTEX_POINT('',#9947);
#2965=VERTEX_POINT('',#9951);
#2966=VERTEX_POINT('',#9955);
#2967=VERTEX_POINT('',#9959);
#2968=VERTEX_POINT('',#9963);
#2969=VERTEX_POINT('',#9964);
#2970=VERTEX_POINT('',#9966);
#2971=VERTEX_POINT('',#9968);
#2972=VERTEX_POINT('',#9972);
#2973=VERTEX_POINT('',#9974);
#2974=VERTEX_POINT('',#9978);
#2975=VERTEX_POINT('',#9980);
#2976=VERTEX_POINT('',#9990);
#2977=VERTEX_POINT('',#9992);
#2978=VERTEX_POINT('',#9996);
#2979=VERTEX_POINT('',#9998);
#2980=VERTEX_POINT('',#10005);
#2981=VERTEX_POINT('',#10007);
#2982=VERTEX_POINT('',#10010);
#2983=VERTEX_POINT('',#10015);
#2984=VERTEX_POINT('',#10017);
#2985=VERTEX_POINT('',#10022);
#2986=VERTEX_POINT('',#10028);
#2987=VERTEX_POINT('',#10030);
#2988=VERTEX_POINT('',#10034);
#2989=VERTEX_POINT('',#10036);
#2990=VERTEX_POINT('',#10043);
#2991=VERTEX_POINT('',#10045);
#2992=VERTEX_POINT('',#10049);
#2993=VERTEX_POINT('',#10051);
#2994=VERTEX_POINT('',#10058);
#2995=VERTEX_POINT('',#10060);
#2996=VERTEX_POINT('',#10063);
#2997=VERTEX_POINT('',#10068);
#2998=VERTEX_POINT('',#10070);
#2999=VERTEX_POINT('',#10075);
#3000=VERTEX_POINT('',#10081);
#3001=VERTEX_POINT('',#10083);
#3002=VERTEX_POINT('',#10087);
#3003=VERTEX_POINT('',#10089);
#3004=VERTEX_POINT('',#10096);
#3005=VERTEX_POINT('',#10098);
#3006=VERTEX_POINT('',#10102);
#3007=VERTEX_POINT('',#10104);
#3008=VERTEX_POINT('',#10111);
#3009=VERTEX_POINT('',#10113);
#3010=VERTEX_POINT('',#10116);
#3011=VERTEX_POINT('',#10121);
#3012=VERTEX_POINT('',#10123);
#3013=VERTEX_POINT('',#10128);
#3014=VERTEX_POINT('',#10134);
#3015=VERTEX_POINT('',#10136);
#3016=VERTEX_POINT('',#10140);
#3017=VERTEX_POINT('',#10142);
#3018=VERTEX_POINT('',#10149);
#3019=VERTEX_POINT('',#10151);
#3020=VERTEX_POINT('',#10155);
#3021=VERTEX_POINT('',#10157);
#3022=VERTEX_POINT('',#10164);
#3023=VERTEX_POINT('',#10166);
#3024=VERTEX_POINT('',#10169);
#3025=VERTEX_POINT('',#10174);
#3026=VERTEX_POINT('',#10176);
#3027=VERTEX_POINT('',#10181);
#3028=VERTEX_POINT('',#10187);
#3029=VERTEX_POINT('',#10189);
#3030=VERTEX_POINT('',#10193);
#3031=VERTEX_POINT('',#10195);
#3032=VERTEX_POINT('',#10202);
#3033=VERTEX_POINT('',#10204);
#3034=VERTEX_POINT('',#10211);
#3035=VERTEX_POINT('',#10213);
#3036=VERTEX_POINT('',#10220);
#3037=VERTEX_POINT('',#10222);
#3038=VERTEX_POINT('',#10227);
#3039=VERTEX_POINT('',#10229);
#3040=VERTEX_POINT('',#10234);
#3041=VERTEX_POINT('',#10236);
#3042=VERTEX_POINT('',#10241);
#3043=VERTEX_POINT('',#10243);
#3044=VERTEX_POINT('',#10248);
#3045=VERTEX_POINT('',#10250);
#3046=VERTEX_POINT('',#10287);
#3047=VERTEX_POINT('',#10289);
#3048=VERTEX_POINT('',#10326);
#3049=VERTEX_POINT('',#10328);
#3050=VERTEX_POINT('',#10365);
#3051=VERTEX_POINT('',#10367);
#3052=VERTEX_POINT('',#10404);
#3053=VERTEX_POINT('',#10405);
#3054=VERTEX_POINT('',#10407);
#3055=VERTEX_POINT('',#10409);
#3056=VERTEX_POINT('',#10413);
#3057=VERTEX_POINT('',#10414);
#3058=VERTEX_POINT('',#10416);
#3059=VERTEX_POINT('',#10420);
#3060=VERTEX_POINT('',#10421);
#3061=VERTEX_POINT('',#10423);
#3062=VERTEX_POINT('',#10436);
#3063=VERTEX_POINT('',#10438);
#3064=VERTEX_POINT('',#10440);
#3065=VERTEX_POINT('',#10442);
#3066=VERTEX_POINT('',#10446);
#3067=VERTEX_POINT('',#10447);
#3068=VERTEX_POINT('',#10452);
#3069=VERTEX_POINT('',#10454);
#3070=VERTEX_POINT('',#10458);
#3071=VERTEX_POINT('',#10460);
#3072=VERTEX_POINT('',#10470);
#3073=VERTEX_POINT('',#10472);
#3074=VERTEX_POINT('',#10476);
#3075=VERTEX_POINT('',#10479);
#3076=VERTEX_POINT('',#10484);
#3077=VERTEX_POINT('',#10486);
#3078=VERTEX_POINT('',#10493);
#3079=VERTEX_POINT('',#10495);
#3080=VERTEX_POINT('',#10499);
#3081=VERTEX_POINT('',#10501);
#3082=VERTEX_POINT('',#10505);
#3083=VERTEX_POINT('',#10507);
#3084=VERTEX_POINT('',#10511);
#3085=VERTEX_POINT('',#10513);
#3086=VERTEX_POINT('',#10517);
#3087=VERTEX_POINT('',#10518);
#3088=VERTEX_POINT('',#10520);
#3089=VERTEX_POINT('',#10522);
#3090=VERTEX_POINT('',#10526);
#3091=VERTEX_POINT('',#10528);
#3092=VERTEX_POINT('',#10532);
#3093=VERTEX_POINT('',#10534);
#3094=VERTEX_POINT('',#10541);
#3095=VERTEX_POINT('',#10542);
#3096=VERTEX_POINT('',#10544);
#3097=VERTEX_POINT('',#10546);
#3098=VERTEX_POINT('',#10550);
#3099=VERTEX_POINT('',#10552);
#3100=VERTEX_POINT('',#10556);
#3101=VERTEX_POINT('',#10558);
#3102=VERTEX_POINT('',#10568);
#3103=VERTEX_POINT('',#10570);
#3104=VERTEX_POINT('',#10574);
#3105=VERTEX_POINT('',#10576);
#3106=VERTEX_POINT('',#10580);
#3107=VERTEX_POINT('',#10582);
#3108=VERTEX_POINT('',#10586);
#3109=VERTEX_POINT('',#10588);
#3110=VERTEX_POINT('',#10592);
#3111=VERTEX_POINT('',#10593);
#3112=VERTEX_POINT('',#10595);
#3113=VERTEX_POINT('',#10597);
#3114=VERTEX_POINT('',#10601);
#3115=VERTEX_POINT('',#10603);
#3116=VERTEX_POINT('',#10607);
#3117=VERTEX_POINT('',#10609);
#3118=VERTEX_POINT('',#10619);
#3119=VERTEX_POINT('',#10621);
#3120=VERTEX_POINT('',#10625);
#3121=VERTEX_POINT('',#10627);
#3122=VERTEX_POINT('',#10631);
#3123=VERTEX_POINT('',#10633);
#3124=VERTEX_POINT('',#10637);
#3125=VERTEX_POINT('',#10639);
#3126=VERTEX_POINT('',#10643);
#3127=VERTEX_POINT('',#10644);
#3128=VERTEX_POINT('',#10646);
#3129=VERTEX_POINT('',#10648);
#3130=VERTEX_POINT('',#10652);
#3131=VERTEX_POINT('',#10654);
#3132=VERTEX_POINT('',#10658);
#3133=VERTEX_POINT('',#10660);
#3134=VERTEX_POINT('',#10667);
#3135=VERTEX_POINT('',#10668);
#3136=VERTEX_POINT('',#10670);
#3137=VERTEX_POINT('',#10672);
#3138=VERTEX_POINT('',#10676);
#3139=VERTEX_POINT('',#10678);
#3140=VERTEX_POINT('',#10682);
#3141=VERTEX_POINT('',#10684);
#3142=VERTEX_POINT('',#10694);
#3143=VERTEX_POINT('',#10695);
#3144=VERTEX_POINT('',#10697);
#3145=VERTEX_POINT('',#10699);
#3146=VERTEX_POINT('',#10703);
#3147=VERTEX_POINT('',#10704);
#3148=VERTEX_POINT('',#10706);
#3149=VERTEX_POINT('',#10708);
#3150=VERTEX_POINT('',#10717);
#3151=VERTEX_POINT('',#10721);
#3152=VERTEX_POINT('',#10723);
#3153=VERTEX_POINT('',#10728);
#3154=VERTEX_POINT('',#10734);
#3155=VERTEX_POINT('',#10735);
#3156=VERTEX_POINT('',#10737);
#3157=VERTEX_POINT('',#10739);
#3158=VERTEX_POINT('',#10743);
#3159=VERTEX_POINT('',#10744);
#3160=VERTEX_POINT('',#10746);
#3161=VERTEX_POINT('',#10748);
#3162=VERTEX_POINT('',#10757);
#3163=VERTEX_POINT('',#10761);
#3164=VERTEX_POINT('',#10763);
#3165=VERTEX_POINT('',#10768);
#3166=VERTEX_POINT('',#10774);
#3167=VERTEX_POINT('',#10775);
#3168=VERTEX_POINT('',#10777);
#3169=VERTEX_POINT('',#10779);
#3170=VERTEX_POINT('',#10783);
#3171=VERTEX_POINT('',#10784);
#3172=VERTEX_POINT('',#10786);
#3173=VERTEX_POINT('',#10788);
#3174=VERTEX_POINT('',#10797);
#3175=VERTEX_POINT('',#10801);
#3176=VERTEX_POINT('',#10803);
#3177=VERTEX_POINT('',#10808);
#3178=VERTEX_POINT('',#10814);
#3179=VERTEX_POINT('',#10815);
#3180=VERTEX_POINT('',#10817);
#3181=VERTEX_POINT('',#10819);
#3182=VERTEX_POINT('',#10823);
#3183=VERTEX_POINT('',#10824);
#3184=VERTEX_POINT('',#10826);
#3185=VERTEX_POINT('',#10828);
#3186=VERTEX_POINT('',#10837);
#3187=VERTEX_POINT('',#10841);
#3188=VERTEX_POINT('',#10843);
#3189=VERTEX_POINT('',#10848);
#3190=VERTEX_POINT('',#10854);
#3191=VERTEX_POINT('',#10856);
#3192=VERTEX_POINT('',#10860);
#3193=VERTEX_POINT('',#10862);
#3194=VERTEX_POINT('',#10866);
#3195=VERTEX_POINT('',#10868);
#3196=VERTEX_POINT('',#10872);
#3197=VERTEX_POINT('',#10874);
#3198=VERTEX_POINT('',#10878);
#3199=VERTEX_POINT('',#10880);
#3200=VERTEX_POINT('',#10884);
#3201=VERTEX_POINT('',#10886);
#3202=VERTEX_POINT('',#10893);
#3203=VERTEX_POINT('',#10895);
#3204=VERTEX_POINT('',#10899);
#3205=VERTEX_POINT('',#10901);
#3206=VERTEX_POINT('',#10905);
#3207=VERTEX_POINT('',#10907);
#3208=VERTEX_POINT('',#10911);
#3209=VERTEX_POINT('',#10913);
#3210=VERTEX_POINT('',#10917);
#3211=VERTEX_POINT('',#10919);
#3212=VERTEX_POINT('',#10923);
#3213=VERTEX_POINT('',#10925);
#3214=VERTEX_POINT('',#10932);
#3215=VERTEX_POINT('',#10934);
#3216=VERTEX_POINT('',#10938);
#3217=VERTEX_POINT('',#10940);
#3218=VERTEX_POINT('',#10943);
#3219=VERTEX_POINT('',#10948);
#3220=VERTEX_POINT('',#10954);
#3221=VERTEX_POINT('',#10955);
#3222=VERTEX_POINT('',#10957);
#3223=VERTEX_POINT('',#10959);
#3224=VERTEX_POINT('',#10963);
#3225=VERTEX_POINT('',#10965);
#3226=VERTEX_POINT('',#10969);
#3227=VERTEX_POINT('',#10971);
#3228=VERTEX_POINT('',#10981);
#3229=VERTEX_POINT('',#10982);
#3230=VERTEX_POINT('',#10984);
#3231=VERTEX_POINT('',#10986);
#3232=VERTEX_POINT('',#10990);
#3233=VERTEX_POINT('',#10992);
#3234=VERTEX_POINT('',#10996);
#3235=VERTEX_POINT('',#10998);
#3236=VERTEX_POINT('',#11008);
#3237=VERTEX_POINT('',#11009);
#3238=VERTEX_POINT('',#11011);
#3239=VERTEX_POINT('',#11013);
#3240=VERTEX_POINT('',#11017);
#3241=VERTEX_POINT('',#11019);
#3242=VERTEX_POINT('',#11023);
#3243=VERTEX_POINT('',#11025);
#3244=VERTEX_POINT('',#11029);
#3245=VERTEX_POINT('',#11031);
#3246=VERTEX_POINT('',#11035);
#3247=VERTEX_POINT('',#11037);
#3248=VERTEX_POINT('',#11046);
#3249=VERTEX_POINT('',#11049);
#3250=VERTEX_POINT('',#11052);
#3251=VERTEX_POINT('',#11056);
#3252=VERTEX_POINT('',#11060);
#3253=VERTEX_POINT('',#11064);
#3254=VERTEX_POINT('',#11067);
#3255=VERTEX_POINT('',#11075);
#3256=VERTEX_POINT('',#11077);
#3257=VERTEX_POINT('',#11081);
#3258=VERTEX_POINT('',#11084);
#3259=VERTEX_POINT('',#11085);
#3260=VERTEX_POINT('',#11087);
#3261=VERTEX_POINT('',#11089);
#3262=VERTEX_POINT('',#11091);
#3263=VERTEX_POINT('',#11093);
#3264=VERTEX_POINT('',#11096);
#3265=VERTEX_POINT('',#11099);
#3266=VERTEX_POINT('',#11100);
#3267=VERTEX_POINT('',#11102);
#3268=VERTEX_POINT('',#11104);
#3269=VERTEX_POINT('',#11106);
#3270=VERTEX_POINT('',#11108);
#3271=VERTEX_POINT('',#11111);
#3272=VERTEX_POINT('',#11126);
#3273=VERTEX_POINT('',#11129);
#3274=VERTEX_POINT('',#11133);
#3275=VERTEX_POINT('',#11138);
#3276=VERTEX_POINT('',#11142);
#3277=VERTEX_POINT('',#11148);
#3278=VERTEX_POINT('',#11150);
#3279=VERTEX_POINT('',#11153);
#3280=VERTEX_POINT('',#11157);
#3281=VERTEX_POINT('',#11160);
#3282=VERTEX_POINT('',#11164);
#3283=VERTEX_POINT('',#11172);
#3284=VERTEX_POINT('',#11173);
#3285=VERTEX_POINT('',#11175);
#3286=VERTEX_POINT('',#11177);
#3287=VERTEX_POINT('',#11179);
#3288=VERTEX_POINT('',#11181);
#3289=VERTEX_POINT('',#11184);
#3290=VERTEX_POINT('',#11187);
#3291=VERTEX_POINT('',#11188);
#3292=VERTEX_POINT('',#11190);
#3293=VERTEX_POINT('',#11192);
#3294=VERTEX_POINT('',#11194);
#3295=VERTEX_POINT('',#11196);
#3296=VERTEX_POINT('',#11199);
#3297=VERTEX_POINT('',#11214);
#3298=VERTEX_POINT('',#11218);
#3299=VERTEX_POINT('',#11220);
#3300=VERTEX_POINT('',#11225);
#3301=VERTEX_POINT('',#11229);
#3302=VERTEX_POINT('',#11233);
#3303=VERTEX_POINT('',#11239);
#3304=VERTEX_POINT('',#11242);
#3305=VERTEX_POINT('',#11246);
#3306=VERTEX_POINT('',#11250);
#3307=VERTEX_POINT('',#11254);
#3308=VERTEX_POINT('',#11257);
#3309=VERTEX_POINT('',#11261);
#3310=VERTEX_POINT('',#11265);
#3311=VERTEX_POINT('',#11270);
#3312=VERTEX_POINT('',#11271);
#3313=VERTEX_POINT('',#11273);
#3314=VERTEX_POINT('',#11275);
#3315=VERTEX_POINT('',#11279);
#3316=VERTEX_POINT('',#11281);
#3317=VERTEX_POINT('',#11285);
#3318=VERTEX_POINT('',#11287);
#3319=VERTEX_POINT('',#11291);
#3320=VERTEX_POINT('',#11293);
#3321=VERTEX_POINT('',#11297);
#3322=VERTEX_POINT('',#11299);
#3323=EDGE_CURVE('',#2836,#2836,#2546,.T.);
#3324=EDGE_CURVE('',#2836,#2837,#1708,.T.);
#3325=EDGE_CURVE('',#2837,#2837,#2547,.T.);
#3326=EDGE_CURVE('',#2838,#2838,#2548,.T.);
#3327=EDGE_CURVE('',#2838,#2839,#1709,.T.);
#3328=EDGE_CURVE('',#2839,#2839,#2549,.T.);
#3329=EDGE_CURVE('',#2840,#2840,#2550,.T.);
#3330=EDGE_CURVE('',#2840,#2841,#1710,.T.);
#3331=EDGE_CURVE('',#2841,#2841,#2551,.T.);
#3332=EDGE_CURVE('',#2842,#2842,#2552,.T.);
#3333=EDGE_CURVE('',#2842,#2843,#1711,.T.);
#3334=EDGE_CURVE('',#2843,#2843,#2553,.T.);
#3335=EDGE_CURVE('',#2844,#2845,#1712,.T.);
#3336=EDGE_CURVE('',#2845,#2846,#1713,.T.);
#3337=EDGE_CURVE('',#2847,#2846,#1714,.T.);
#3338=EDGE_CURVE('',#2844,#2847,#1715,.T.);
#3339=EDGE_CURVE('',#2848,#2844,#1716,.T.);
#3340=EDGE_CURVE('',#2849,#2847,#1717,.T.);
#3341=EDGE_CURVE('',#2848,#2849,#1718,.T.);
#3342=EDGE_CURVE('',#2850,#2848,#1719,.T.);
#3343=EDGE_CURVE('',#2851,#2849,#1720,.T.);
#3344=EDGE_CURVE('',#2850,#2851,#1721,.T.);
#3345=EDGE_CURVE('',#2845,#2850,#1722,.T.);
#3346=EDGE_CURVE('',#2846,#2851,#1723,.T.);
#3347=EDGE_CURVE('',#2852,#2852,#2554,.T.);
#3348=EDGE_CURVE('',#2852,#2853,#1724,.T.);
#3349=EDGE_CURVE('',#2853,#2853,#2555,.T.);
#3350=EDGE_CURVE('',#2854,#2854,#2556,.T.);
#3351=EDGE_CURVE('',#2854,#2855,#1725,.T.);
#3352=EDGE_CURVE('',#2855,#2855,#2557,.T.);
#3353=EDGE_CURVE('',#2856,#2856,#2558,.T.);
#3354=EDGE_CURVE('',#2857,#2857,#2559,.T.);
#3355=EDGE_CURVE('',#2857,#2858,#1726,.T.);
#3356=EDGE_CURVE('',#2858,#2858,#2560,.T.);
#3357=EDGE_CURVE('',#2859,#2859,#2561,.T.);
#3358=EDGE_CURVE('',#2860,#2860,#2562,.T.);
#3359=EDGE_CURVE('',#2860,#2856,#1727,.T.);
#3360=EDGE_CURVE('',#2861,#2861,#2563,.T.);
#3361=EDGE_CURVE('',#2861,#2859,#1728,.T.);
#3362=EDGE_CURVE('',#2862,#2863,#1729,.T.);
#3363=EDGE_CURVE('',#2863,#2864,#1730,.T.);
#3364=EDGE_CURVE('',#2865,#2864,#1731,.T.);
#3365=EDGE_CURVE('',#2862,#2865,#1732,.T.);
#3366=EDGE_CURVE('',#2866,#2862,#1733,.T.);
#3367=EDGE_CURVE('',#2867,#2865,#1734,.T.);
#3368=EDGE_CURVE('',#2866,#2867,#1735,.T.);
#3369=EDGE_CURVE('',#2868,#2866,#1736,.T.);
#3370=EDGE_CURVE('',#2869,#2867,#1737,.T.);
#3371=EDGE_CURVE('',#2868,#2869,#1738,.T.);
#3372=EDGE_CURVE('',#2863,#2868,#1739,.T.);
#3373=EDGE_CURVE('',#2864,#2869,#1740,.T.);
#3374=EDGE_CURVE('',#2870,#2870,#2564,.T.);
#3375=EDGE_CURVE('',#2870,#2871,#1741,.T.);
#3376=EDGE_CURVE('',#2871,#2871,#2565,.T.);
#3377=EDGE_CURVE('',#2872,#2872,#2566,.T.);
#3378=EDGE_CURVE('',#2872,#2873,#1742,.T.);
#3379=EDGE_CURVE('',#2873,#2873,#2567,.T.);
#3380=EDGE_CURVE('',#2874,#2874,#2568,.T.);
#3381=EDGE_CURVE('',#2875,#2875,#2569,.T.);
#3382=EDGE_CURVE('',#2875,#2876,#1743,.T.);
#3383=EDGE_CURVE('',#2876,#2876,#2570,.T.);
#3384=EDGE_CURVE('',#2877,#2877,#2571,.T.);
#3385=EDGE_CURVE('',#2878,#2878,#2572,.T.);
#3386=EDGE_CURVE('',#2878,#2874,#1744,.T.);
#3387=EDGE_CURVE('',#2879,#2879,#2573,.T.);
#3388=EDGE_CURVE('',#2879,#2877,#1745,.T.);
#3389=EDGE_CURVE('',#2880,#2881,#1746,.T.);
#3390=EDGE_CURVE('',#2881,#2882,#1747,.T.);
#3391=EDGE_CURVE('',#2883,#2882,#1748,.T.);
#3392=EDGE_CURVE('',#2880,#2883,#1749,.T.);
#3393=EDGE_CURVE('',#2884,#2880,#1750,.T.);
#3394=EDGE_CURVE('',#2885,#2883,#1751,.T.);
#3395=EDGE_CURVE('',#2884,#2885,#1752,.T.);
#3396=EDGE_CURVE('',#2886,#2884,#1753,.T.);
#3397=EDGE_CURVE('',#2887,#2885,#1754,.T.);
#3398=EDGE_CURVE('',#2886,#2887,#1755,.T.);
#3399=EDGE_CURVE('',#2881,#2886,#1756,.T.);
#3400=EDGE_CURVE('',#2882,#2887,#1757,.T.);
#3401=EDGE_CURVE('',#2888,#2889,#1758,.T.);
#3402=EDGE_CURVE('',#2888,#2889,#2574,.T.);
#3403=EDGE_CURVE('',#2890,#2888,#1759,.T.);
#3404=EDGE_CURVE('',#2890,#2888,#2575,.T.);
#3405=EDGE_CURVE('',#2891,#2892,#1760,.T.);
#3406=EDGE_CURVE('',#2892,#2891,#2576,.T.);
#3407=EDGE_CURVE('',#2889,#2893,#1761,.T.);
#3408=EDGE_CURVE('',#2894,#2888,#1762,.T.);
#3409=EDGE_CURVE('',#2895,#2894,#253,.T.);
#3410=EDGE_CURVE('',#2896,#2895,#254,.T.);
#3411=EDGE_CURVE('',#2896,#2897,#1763,.T.);
#3412=EDGE_CURVE('',#2898,#2897,#224,.T.);
#3413=EDGE_CURVE('',#2892,#2898,#225,.T.);
#3414=EDGE_CURVE('',#2899,#2891,#226,.T.);
#3415=EDGE_CURVE('',#2900,#2899,#227,.T.);
#3416=EDGE_CURVE('',#2900,#2901,#2577,.T.);
#3417=EDGE_CURVE('',#2897,#2901,#228,.T.);
#3418=EDGE_CURVE('',#2893,#2896,#255,.T.);
#3419=EDGE_CURVE('',#2895,#2890,#256,.T.);
#3420=EDGE_CURVE('',#2888,#2895,#257,.T.);
#3421=EDGE_CURVE('',#2902,#2896,#258,.T.);
#3422=EDGE_CURVE('',#2889,#2902,#2578,.T.);
#3423=EDGE_CURVE('',#2896,#2889,#259,.T.);
#3424=EDGE_CURVE('',#2901,#2900,#1764,.T.);
#3425=EDGE_CURVE('',#2889,#2902,#1765,.T.);
#3426=EDGE_CURVE('',#2888,#2894,#2579,.T.);
#3427=EDGE_CURVE('',#2889,#2888,#2580,.T.);
#3428=EDGE_CURVE('',#2896,#2903,#1766,.T.);
#3429=EDGE_CURVE('',#2903,#2903,#2581,.T.);
#3430=EDGE_CURVE('',#2893,#2889,#2582,.T.);
#3431=EDGE_CURVE('',#2904,#2904,#2583,.T.);
#3432=EDGE_CURVE('',#2904,#2905,#1767,.T.);
#3433=EDGE_CURVE('',#2905,#2905,#2584,.T.);
#3434=EDGE_CURVE('',#2906,#2907,#229,.T.);
#3435=EDGE_CURVE('',#2908,#2906,#230,.T.);
#3436=EDGE_CURVE('',#2908,#2909,#1768,.T.);
#3437=EDGE_CURVE('',#2909,#2909,#2585,.T.);
#3438=EDGE_CURVE('',#2907,#2908,#231,.T.);
#3439=EDGE_CURVE('',#2910,#2910,#2586,.T.);
#3440=EDGE_CURVE('',#2910,#2911,#1769,.T.);
#3441=EDGE_CURVE('',#2911,#2911,#2587,.T.);
#3442=EDGE_CURVE('',#2912,#2912,#2588,.T.);
#3443=EDGE_CURVE('',#2912,#2913,#1770,.T.);
#3444=EDGE_CURVE('',#2914,#2913,#232,.T.);
#3445=EDGE_CURVE('',#2913,#2914,#233,.T.);
#3446=EDGE_CURVE('',#2915,#2915,#2589,.T.);
#3447=EDGE_CURVE('',#2915,#2916,#1771,.T.);
#3448=EDGE_CURVE('',#2916,#2916,#2590,.T.);
#3449=EDGE_CURVE('',#2917,#2918,#234,.T.);
#3450=EDGE_CURVE('',#2919,#2917,#235,.T.);
#3451=EDGE_CURVE('',#2919,#2920,#1772,.T.);
#3452=EDGE_CURVE('',#2920,#2920,#2591,.T.);
#3453=EDGE_CURVE('',#2918,#2919,#236,.T.);
#3454=EDGE_CURVE('',#2921,#2921,#2592,.T.);
#3455=EDGE_CURVE('',#2921,#2922,#1773,.T.);
#3456=EDGE_CURVE('',#2922,#2922,#2593,.T.);
#3457=EDGE_CURVE('',#2923,#2923,#2594,.T.);
#3458=EDGE_CURVE('',#2923,#2924,#1774,.T.);
#3459=EDGE_CURVE('',#2925,#2924,#237,.T.);
#3460=EDGE_CURVE('',#2924,#2925,#238,.T.);
#3461=EDGE_CURVE('',#2926,#2926,#2595,.T.);
#3462=EDGE_CURVE('',#2926,#2927,#1775,.T.);
#3463=EDGE_CURVE('',#2927,#2927,#2596,.T.);
#3464=EDGE_CURVE('',#2928,#2929,#239,.T.);
#3465=EDGE_CURVE('',#2930,#2928,#240,.T.);
#3466=EDGE_CURVE('',#2930,#2931,#1776,.T.);
#3467=EDGE_CURVE('',#2931,#2931,#2597,.T.);
#3468=EDGE_CURVE('',#2929,#2930,#241,.T.);
#3469=EDGE_CURVE('',#2932,#2932,#2598,.T.);
#3470=EDGE_CURVE('',#2932,#2933,#1777,.T.);
#3471=EDGE_CURVE('',#2933,#2933,#2599,.T.);
#3472=EDGE_CURVE('',#2934,#2934,#2600,.T.);
#3473=EDGE_CURVE('',#2934,#2935,#1778,.T.);
#3474=EDGE_CURVE('',#2936,#2935,#242,.T.);
#3475=EDGE_CURVE('',#2935,#2936,#243,.T.);
#3476=EDGE_CURVE('',#2937,#2937,#2601,.T.);
#3477=EDGE_CURVE('',#2937,#2938,#1779,.T.);
#3478=EDGE_CURVE('',#2938,#2938,#2602,.T.);
#3479=EDGE_CURVE('',#2939,#2940,#244,.T.);
#3480=EDGE_CURVE('',#2941,#2939,#245,.T.);
#3481=EDGE_CURVE('',#2941,#2942,#1780,.T.);
#3482=EDGE_CURVE('',#2942,#2942,#2603,.T.);
#3483=EDGE_CURVE('',#2940,#2941,#246,.T.);
#3484=EDGE_CURVE('',#2943,#2943,#2604,.T.);
#3485=EDGE_CURVE('',#2943,#2944,#1781,.T.);
#3486=EDGE_CURVE('',#2944,#2944,#2605,.T.);
#3487=EDGE_CURVE('',#2945,#2945,#2606,.T.);
#3488=EDGE_CURVE('',#2945,#2946,#1782,.T.);
#3489=EDGE_CURVE('',#2947,#2946,#247,.T.);
#3490=EDGE_CURVE('',#2946,#2947,#248,.T.);
#3491=EDGE_CURVE('',#2948,#2948,#2607,.T.);
#3492=EDGE_CURVE('',#2948,#2949,#1783,.T.);
#3493=EDGE_CURVE('',#2949,#2949,#2608,.T.);
#3494=EDGE_CURVE('',#2950,#2950,#2609,.T.);
#3495=EDGE_CURVE('',#2950,#2941,#1784,.T.);
#3496=EDGE_CURVE('',#2940,#2930,#1785,.T.);
#3497=EDGE_CURVE('',#2929,#2898,#1786,.T.);
#3498=EDGE_CURVE('',#2899,#2919,#1787,.T.);
#3499=EDGE_CURVE('',#2918,#2908,#1788,.T.);
#3500=EDGE_CURVE('',#2907,#2951,#1789,.T.);
#3501=EDGE_CURVE('',#2951,#2951,#2610,.T.);
#3502=EDGE_CURVE('',#2952,#2952,#2611,.T.);
#3503=EDGE_CURVE('',#2952,#2953,#1790,.T.);
#3504=EDGE_CURVE('',#2953,#2953,#2612,.T.);
#3505=EDGE_CURVE('',#2954,#2954,#2613,.T.);
#3506=EDGE_CURVE('',#2955,#2955,#2614,.T.);
#3507=EDGE_CURVE('',#2955,#2956,#1791,.T.);
#3508=EDGE_CURVE('',#2956,#2956,#2615,.T.);
#3509=EDGE_CURVE('',#2957,#2957,#2616,.T.);
#3510=EDGE_CURVE('',#2958,#2958,#2617,.T.);
#3511=EDGE_CURVE('',#2958,#2959,#1792,.T.);
#3512=EDGE_CURVE('',#2959,#2959,#2618,.T.);
#3513=EDGE_CURVE('',#2960,#2960,#2619,.T.);
#3514=EDGE_CURVE('',#2961,#2961,#2620,.T.);
#3515=EDGE_CURVE('',#2961,#2962,#1793,.T.);
#3516=EDGE_CURVE('',#2962,#2962,#2621,.T.);
#3517=EDGE_CURVE('',#2963,#2963,#2622,.T.);
#3518=EDGE_CURVE('',#2964,#2964,#2623,.T.);
#3519=EDGE_CURVE('',#2964,#2954,#1794,.T.);
#3520=EDGE_CURVE('',#2965,#2965,#2624,.T.);
#3521=EDGE_CURVE('',#2965,#2957,#1795,.T.);
#3522=EDGE_CURVE('',#2966,#2966,#2625,.T.);
#3523=EDGE_CURVE('',#2966,#2960,#1796,.T.);
#3524=EDGE_CURVE('',#2967,#2967,#2626,.T.);
#3525=EDGE_CURVE('',#2967,#2963,#1797,.T.);
#3526=EDGE_CURVE('',#2968,#2969,#1798,.T.);
#3527=EDGE_CURVE('',#2969,#2970,#1799,.T.);
#3528=EDGE_CURVE('',#2971,#2970,#1800,.T.);
#3529=EDGE_CURVE('',#2968,#2971,#1801,.T.);
#3530=EDGE_CURVE('',#2972,#2968,#1802,.T.);
#3531=EDGE_CURVE('',#2973,#2971,#1803,.T.);
#3532=EDGE_CURVE('',#2972,#2973,#1804,.T.);
#3533=EDGE_CURVE('',#2974,#2972,#1805,.T.);
#3534=EDGE_CURVE('',#2975,#2973,#1806,.T.);
#3535=EDGE_CURVE('',#2974,#2975,#1807,.T.);
#3536=EDGE_CURVE('',#2969,#2974,#1808,.T.);
#3537=EDGE_CURVE('',#2970,#2975,#1809,.T.);
#3538=EDGE_CURVE('',#2976,#2976,#2627,.T.);
#3539=EDGE_CURVE('',#2976,#2977,#1810,.T.);
#3540=EDGE_CURVE('',#2977,#2977,#2628,.T.);
#3541=EDGE_CURVE('',#2978,#2978,#2629,.T.);
#3542=EDGE_CURVE('',#2978,#2979,#1811,.T.);
#3543=EDGE_CURVE('',#2979,#2979,#2630,.T.);
#3544=EDGE_CURVE('',#2980,#2980,#2631,.T.);
#3545=EDGE_CURVE('',#2981,#2981,#2632,.T.);
#3546=EDGE_CURVE('',#2982,#2982,#2633,.T.);
#3547=EDGE_CURVE('',#2982,#2980,#1812,.T.);
#3548=EDGE_CURVE('',#2983,#2983,#2634,.T.);
#3549=EDGE_CURVE('',#2984,#2984,#2635,.T.);
#3550=EDGE_CURVE('',#2981,#2983,#1813,.T.);
#3551=EDGE_CURVE('',#2984,#2985,#1814,.T.);
#3552=EDGE_CURVE('',#2985,#2985,#2636,.T.);
#3553=EDGE_CURVE('',#2986,#2986,#2637,.T.);
#3554=EDGE_CURVE('',#2986,#2987,#1815,.T.);
#3555=EDGE_CURVE('',#2987,#2987,#2638,.T.);
#3556=EDGE_CURVE('',#2988,#2988,#2639,.T.);
#3557=EDGE_CURVE('',#2988,#2989,#1816,.T.);
#3558=EDGE_CURVE('',#2989,#2989,#2640,.T.);
#3559=EDGE_CURVE('',#2990,#2990,#2641,.T.);
#3560=EDGE_CURVE('',#2990,#2991,#1817,.T.);
#3561=EDGE_CURVE('',#2991,#2991,#2642,.T.);
#3562=EDGE_CURVE('',#2992,#2992,#2643,.T.);
#3563=EDGE_CURVE('',#2992,#2993,#1818,.T.);
#3564=EDGE_CURVE('',#2993,#2993,#2644,.T.);
#3565=EDGE_CURVE('',#2994,#2994,#2645,.T.);
#3566=EDGE_CURVE('',#2995,#2995,#2646,.T.);
#3567=EDGE_CURVE('',#2996,#2996,#2647,.T.);
#3568=EDGE_CURVE('',#2996,#2994,#1819,.T.);
#3569=EDGE_CURVE('',#2997,#2997,#2648,.T.);
#3570=EDGE_CURVE('',#2998,#2998,#2649,.T.);
#3571=EDGE_CURVE('',#2995,#2997,#1820,.T.);
#3572=EDGE_CURVE('',#2998,#2999,#1821,.T.);
#3573=EDGE_CURVE('',#2999,#2999,#2650,.T.);
#3574=EDGE_CURVE('',#3000,#3000,#2651,.T.);
#3575=EDGE_CURVE('',#3000,#3001,#1822,.T.);
#3576=EDGE_CURVE('',#3001,#3001,#2652,.T.);
#3577=EDGE_CURVE('',#3002,#3002,#2653,.T.);
#3578=EDGE_CURVE('',#3002,#3003,#1823,.T.);
#3579=EDGE_CURVE('',#3003,#3003,#2654,.T.);
#3580=EDGE_CURVE('',#3004,#3004,#2655,.T.);
#3581=EDGE_CURVE('',#3004,#3005,#1824,.T.);
#3582=EDGE_CURVE('',#3005,#3005,#2656,.T.);
#3583=EDGE_CURVE('',#3006,#3006,#2657,.T.);
#3584=EDGE_CURVE('',#3006,#3007,#1825,.T.);
#3585=EDGE_CURVE('',#3007,#3007,#2658,.T.);
#3586=EDGE_CURVE('',#3008,#3008,#2659,.T.);
#3587=EDGE_CURVE('',#3009,#3009,#2660,.T.);
#3588=EDGE_CURVE('',#3010,#3010,#2661,.T.);
#3589=EDGE_CURVE('',#3010,#3008,#1826,.T.);
#3590=EDGE_CURVE('',#3011,#3011,#2662,.T.);
#3591=EDGE_CURVE('',#3012,#3012,#2663,.T.);
#3592=EDGE_CURVE('',#3009,#3011,#1827,.T.);
#3593=EDGE_CURVE('',#3012,#3013,#1828,.T.);
#3594=EDGE_CURVE('',#3013,#3013,#2664,.T.);
#3595=EDGE_CURVE('',#3014,#3014,#2665,.T.);
#3596=EDGE_CURVE('',#3014,#3015,#1829,.T.);
#3597=EDGE_CURVE('',#3015,#3015,#2666,.T.);
#3598=EDGE_CURVE('',#3016,#3016,#2667,.T.);
#3599=EDGE_CURVE('',#3016,#3017,#1830,.T.);
#3600=EDGE_CURVE('',#3017,#3017,#2668,.T.);
#3601=EDGE_CURVE('',#3018,#3018,#2669,.T.);
#3602=EDGE_CURVE('',#3018,#3019,#1831,.T.);
#3603=EDGE_CURVE('',#3019,#3019,#2670,.T.);
#3604=EDGE_CURVE('',#3020,#3020,#2671,.T.);
#3605=EDGE_CURVE('',#3020,#3021,#1832,.T.);
#3606=EDGE_CURVE('',#3021,#3021,#2672,.T.);
#3607=EDGE_CURVE('',#3022,#3022,#2673,.T.);
#3608=EDGE_CURVE('',#3023,#3023,#2674,.T.);
#3609=EDGE_CURVE('',#3024,#3024,#2675,.T.);
#3610=EDGE_CURVE('',#3024,#3022,#1833,.T.);
#3611=EDGE_CURVE('',#3025,#3025,#2676,.T.);
#3612=EDGE_CURVE('',#3026,#3026,#2677,.T.);
#3613=EDGE_CURVE('',#3023,#3025,#1834,.T.);
#3614=EDGE_CURVE('',#3026,#3027,#1835,.T.);
#3615=EDGE_CURVE('',#3027,#3027,#2678,.T.);
#3616=EDGE_CURVE('',#3028,#3028,#2679,.T.);
#3617=EDGE_CURVE('',#3028,#3029,#1836,.T.);
#3618=EDGE_CURVE('',#3029,#3029,#2680,.T.);
#3619=EDGE_CURVE('',#3030,#3030,#2681,.T.);
#3620=EDGE_CURVE('',#3030,#3031,#1837,.T.);
#3621=EDGE_CURVE('',#3031,#3031,#2682,.T.);
#3622=EDGE_CURVE('',#3032,#3032,#2683,.T.);
#3623=EDGE_CURVE('',#3032,#3033,#1838,.T.);
#3624=EDGE_CURVE('',#3033,#3033,#2684,.T.);
#3625=EDGE_CURVE('',#3034,#3034,#2685,.T.);
#3626=EDGE_CURVE('',#3034,#3035,#1839,.T.);
#3627=EDGE_CURVE('',#3035,#3035,#2686,.T.);
#3628=EDGE_CURVE('',#3036,#3036,#2687,.T.);
#3629=EDGE_CURVE('',#3036,#3037,#1840,.T.);
#3630=EDGE_CURVE('',#3037,#3037,#2688,.T.);
#3631=EDGE_CURVE('',#3038,#3038,#2689,.T.);
#3632=EDGE_CURVE('',#3038,#3039,#1841,.T.);
#3633=EDGE_CURVE('',#3039,#3039,#2690,.T.);
#3634=EDGE_CURVE('',#3040,#3040,#2691,.T.);
#3635=EDGE_CURVE('',#3040,#3041,#1842,.T.);
#3636=EDGE_CURVE('',#3041,#3041,#2692,.T.);
#3637=EDGE_CURVE('',#3042,#3042,#2693,.T.);
#3638=EDGE_CURVE('',#3042,#3043,#1843,.T.);
#3639=EDGE_CURVE('',#3043,#3043,#2694,.T.);
#3640=EDGE_CURVE('',#3044,#3044,#2695,.T.);
#3641=EDGE_CURVE('',#3044,#3045,#1844,.T.);
#3642=EDGE_CURVE('',#3045,#3045,#249,.T.);
#3643=EDGE_CURVE('',#3046,#3046,#2696,.T.);
#3644=EDGE_CURVE('',#3046,#3047,#1845,.T.);
#3645=EDGE_CURVE('',#3047,#3047,#250,.T.);
#3646=EDGE_CURVE('',#3048,#3048,#2697,.T.);
#3647=EDGE_CURVE('',#3048,#3049,#1846,.T.);
#3648=EDGE_CURVE('',#3049,#3049,#251,.T.);
#3649=EDGE_CURVE('',#3050,#3050,#2698,.T.);
#3650=EDGE_CURVE('',#3050,#3051,#1847,.T.);
#3651=EDGE_CURVE('',#3051,#3051,#252,.T.);
#3652=EDGE_CURVE('',#3052,#3053,#1848,.T.);
#3653=EDGE_CURVE('',#3054,#3052,#1849,.T.);
#3654=EDGE_CURVE('',#3055,#3054,#1850,.T.);
#3655=EDGE_CURVE('',#3055,#3053,#1851,.T.);
#3656=EDGE_CURVE('',#3056,#3057,#2699,.T.);
#3657=EDGE_CURVE('',#3058,#3056,#1852,.T.);
#3658=EDGE_CURVE('',#3057,#3058,#1853,.T.);
#3659=EDGE_CURVE('',#3059,#3060,#2700,.T.);
#3660=EDGE_CURVE('',#3061,#3059,#1854,.T.);
#3661=EDGE_CURVE('',#3061,#3060,#1855,.T.);
#3662=EDGE_CURVE('',#3053,#3059,#2701,.T.);
#3663=EDGE_CURVE('',#3059,#3055,#1856,.T.);
#3664=EDGE_CURVE('',#3060,#3056,#1857,.T.);
#3665=EDGE_CURVE('',#3058,#3061,#1858,.T.);
#3666=EDGE_CURVE('',#3057,#3052,#2702,.T.);
#3667=EDGE_CURVE('',#3054,#3057,#1859,.T.);
#3668=EDGE_CURVE('',#3059,#3062,#1860,.T.);
#3669=EDGE_CURVE('',#3063,#3062,#1861,.T.);
#3670=EDGE_CURVE('',#3064,#3063,#1862,.T.);
#3671=EDGE_CURVE('',#3065,#3064,#1863,.T.);
#3672=EDGE_CURVE('',#3065,#3057,#1864,.T.);
#3673=EDGE_CURVE('',#3066,#3067,#1865,.T.);
#3674=EDGE_CURVE('',#3066,#3064,#1866,.T.);
#3675=EDGE_CURVE('',#3067,#3063,#1867,.T.);
#3676=EDGE_CURVE('',#3067,#3068,#2703,.T.);
#3677=EDGE_CURVE('',#3062,#3069,#1868,.T.);
#3678=EDGE_CURVE('',#3068,#3069,#1869,.T.);
#3679=EDGE_CURVE('',#3068,#3070,#1870,.T.);
#3680=EDGE_CURVE('',#3069,#3071,#1871,.T.);
#3681=EDGE_CURVE('',#3070,#3071,#1872,.T.);
#3682=EDGE_CURVE('',#3070,#3066,#2704,.T.);
#3683=EDGE_CURVE('',#3071,#3065,#1873,.T.);
#3684=EDGE_CURVE('',#3065,#3057,#1874,.T.);
#3685=EDGE_CURVE('',#3059,#3062,#1875,.T.);
#3686=EDGE_CURVE('',#3072,#3072,#2705,.T.);
#3687=EDGE_CURVE('',#3072,#3073,#1876,.T.);
#3688=EDGE_CURVE('',#3073,#3073,#2706,.T.);
#3689=EDGE_CURVE('',#3074,#3074,#2707,.T.);
#3690=EDGE_CURVE('',#3074,#3062,#1877,.T.);
#3691=EDGE_CURVE('',#3065,#3075,#1878,.T.);
#3692=EDGE_CURVE('',#3075,#3075,#2708,.T.);
#3693=EDGE_CURVE('',#3076,#3076,#2709,.T.);
#3694=EDGE_CURVE('',#3076,#3077,#1879,.T.);
#3695=EDGE_CURVE('',#3077,#3077,#2710,.T.);
#3696=EDGE_CURVE('',#3078,#3078,#2711,.T.);
#3697=EDGE_CURVE('',#3078,#3079,#1880,.T.);
#3698=EDGE_CURVE('',#3079,#3079,#2712,.T.);
#3699=EDGE_CURVE('',#3080,#3080,#2713,.T.);
#3700=EDGE_CURVE('',#3080,#3081,#1881,.T.);
#3701=EDGE_CURVE('',#3081,#3081,#2714,.T.);
#3702=EDGE_CURVE('',#3082,#3082,#2715,.T.);
#3703=EDGE_CURVE('',#3082,#3083,#1882,.T.);
#3704=EDGE_CURVE('',#3083,#3083,#2716,.T.);
#3705=EDGE_CURVE('',#3084,#3084,#2717,.T.);
#3706=EDGE_CURVE('',#3084,#3085,#1883,.T.);
#3707=EDGE_CURVE('',#3085,#3085,#2718,.T.);
#3708=EDGE_CURVE('',#3086,#3087,#1884,.T.);
#3709=EDGE_CURVE('',#3088,#3086,#1885,.T.);
#3710=EDGE_CURVE('',#3089,#3088,#1886,.T.);
#3711=EDGE_CURVE('',#3089,#3087,#1887,.T.);
#3712=EDGE_CURVE('',#3087,#3090,#1888,.T.);
#3713=EDGE_CURVE('',#3091,#3089,#1889,.T.);
#3714=EDGE_CURVE('',#3091,#3090,#1890,.T.);
#3715=EDGE_CURVE('',#3090,#3092,#1891,.T.);
#3716=EDGE_CURVE('',#3093,#3091,#1892,.T.);
#3717=EDGE_CURVE('',#3093,#3092,#1893,.T.);
#3718=EDGE_CURVE('',#3092,#3086,#1894,.T.);
#3719=EDGE_CURVE('',#3088,#3093,#1895,.T.);
#3720=EDGE_CURVE('',#3094,#3095,#1896,.T.);
#3721=EDGE_CURVE('',#3095,#3096,#1897,.T.);
#3722=EDGE_CURVE('',#3097,#3096,#1898,.T.);
#3723=EDGE_CURVE('',#3094,#3097,#1899,.T.);
#3724=EDGE_CURVE('',#3098,#3094,#1900,.T.);
#3725=EDGE_CURVE('',#3099,#3097,#1901,.T.);
#3726=EDGE_CURVE('',#3098,#3099,#1902,.T.);
#3727=EDGE_CURVE('',#3100,#3098,#1903,.T.);
#3728=EDGE_CURVE('',#3101,#3099,#1904,.T.);
#3729=EDGE_CURVE('',#3100,#3101,#1905,.T.);
#3730=EDGE_CURVE('',#3095,#3100,#1906,.T.);
#3731=EDGE_CURVE('',#3096,#3101,#1907,.T.);
#3732=EDGE_CURVE('',#3102,#3102,#2719,.T.);
#3733=EDGE_CURVE('',#3102,#3103,#1908,.T.);
#3734=EDGE_CURVE('',#3103,#3103,#2720,.T.);
#3735=EDGE_CURVE('',#3104,#3104,#2721,.T.);
#3736=EDGE_CURVE('',#3104,#3105,#1909,.T.);
#3737=EDGE_CURVE('',#3105,#3105,#2722,.T.);
#3738=EDGE_CURVE('',#3106,#3106,#2723,.T.);
#3739=EDGE_CURVE('',#3106,#3107,#1910,.T.);
#3740=EDGE_CURVE('',#3107,#3107,#2724,.T.);
#3741=EDGE_CURVE('',#3108,#3108,#2725,.T.);
#3742=EDGE_CURVE('',#3108,#3109,#1911,.T.);
#3743=EDGE_CURVE('',#3109,#3109,#2726,.T.);
#3744=EDGE_CURVE('',#3110,#3111,#1912,.T.);
#3745=EDGE_CURVE('',#3111,#3112,#1913,.T.);
#3746=EDGE_CURVE('',#3113,#3112,#1914,.T.);
#3747=EDGE_CURVE('',#3110,#3113,#1915,.T.);
#3748=EDGE_CURVE('',#3114,#3110,#1916,.T.);
#3749=EDGE_CURVE('',#3115,#3113,#1917,.T.);
#3750=EDGE_CURVE('',#3114,#3115,#1918,.T.);
#3751=EDGE_CURVE('',#3116,#3114,#1919,.T.);
#3752=EDGE_CURVE('',#3117,#3115,#1920,.T.);
#3753=EDGE_CURVE('',#3116,#3117,#1921,.T.);
#3754=EDGE_CURVE('',#3111,#3116,#1922,.T.);
#3755=EDGE_CURVE('',#3112,#3117,#1923,.T.);
#3756=EDGE_CURVE('',#3118,#3118,#2727,.T.);
#3757=EDGE_CURVE('',#3118,#3119,#1924,.T.);
#3758=EDGE_CURVE('',#3119,#3119,#2728,.T.);
#3759=EDGE_CURVE('',#3120,#3120,#2729,.T.);
#3760=EDGE_CURVE('',#3120,#3121,#1925,.T.);
#3761=EDGE_CURVE('',#3121,#3121,#2730,.T.);
#3762=EDGE_CURVE('',#3122,#3122,#2731,.T.);
#3763=EDGE_CURVE('',#3122,#3123,#1926,.T.);
#3764=EDGE_CURVE('',#3123,#3123,#2732,.T.);
#3765=EDGE_CURVE('',#3124,#3124,#2733,.T.);
#3766=EDGE_CURVE('',#3124,#3125,#1927,.T.);
#3767=EDGE_CURVE('',#3125,#3125,#2734,.T.);
#3768=EDGE_CURVE('',#3126,#3127,#1928,.T.);
#3769=EDGE_CURVE('',#3128,#3126,#1929,.T.);
#3770=EDGE_CURVE('',#3129,#3128,#1930,.T.);
#3771=EDGE_CURVE('',#3129,#3127,#1931,.T.);
#3772=EDGE_CURVE('',#3127,#3130,#1932,.T.);
#3773=EDGE_CURVE('',#3131,#3129,#1933,.T.);
#3774=EDGE_CURVE('',#3131,#3130,#1934,.T.);
#3775=EDGE_CURVE('',#3130,#3132,#1935,.T.);
#3776=EDGE_CURVE('',#3133,#3131,#1936,.T.);
#3777=EDGE_CURVE('',#3133,#3132,#1937,.T.);
#3778=EDGE_CURVE('',#3132,#3126,#1938,.T.);
#3779=EDGE_CURVE('',#3128,#3133,#1939,.T.);
#3780=EDGE_CURVE('',#3134,#3135,#1940,.T.);
#3781=EDGE_CURVE('',#3135,#3136,#1941,.T.);
#3782=EDGE_CURVE('',#3137,#3136,#1942,.T.);
#3783=EDGE_CURVE('',#3134,#3137,#1943,.T.);
#3784=EDGE_CURVE('',#3138,#3134,#1944,.T.);
#3785=EDGE_CURVE('',#3139,#3137,#1945,.T.);
#3786=EDGE_CURVE('',#3138,#3139,#1946,.T.);
#3787=EDGE_CURVE('',#3140,#3138,#1947,.T.);
#3788=EDGE_CURVE('',#3141,#3139,#1948,.T.);
#3789=EDGE_CURVE('',#3140,#3141,#1949,.T.);
#3790=EDGE_CURVE('',#3135,#3140,#1950,.T.);
#3791=EDGE_CURVE('',#3136,#3141,#1951,.T.);
#3792=EDGE_CURVE('',#3142,#3143,#1952,.T.);
#3793=EDGE_CURVE('',#3142,#3144,#1953,.T.);
#3794=EDGE_CURVE('',#3145,#3144,#1954,.T.);
#3795=EDGE_CURVE('',#3143,#3145,#1955,.T.);
#3796=EDGE_CURVE('',#3146,#3147,#1956,.T.);
#3797=EDGE_CURVE('',#3148,#3146,#1957,.T.);
#3798=EDGE_CURVE('',#3149,#3148,#1958,.T.);
#3799=EDGE_CURVE('',#3149,#3147,#1959,.T.);
#3800=EDGE_CURVE('',#3147,#3142,#2735,.T.);
#3801=EDGE_CURVE('',#3144,#3149,#2736,.T.);
#3802=EDGE_CURVE('',#3148,#3146,#2737,.T.);
#3803=EDGE_CURVE('',#3150,#3145,#2738,.T.);
#3804=EDGE_CURVE('',#3143,#3150,#2739,.T.);
#3805=EDGE_CURVE('',#3151,#3151,#2740,.T.);
#3806=EDGE_CURVE('',#3152,#3152,#2741,.T.);
#3807=EDGE_CURVE('',#3151,#3150,#1960,.T.);
#3808=EDGE_CURVE('',#3153,#3153,#2742,.T.);
#3809=EDGE_CURVE('',#3153,#3152,#1961,.T.);
#3810=EDGE_CURVE('',#3154,#3155,#1962,.T.);
#3811=EDGE_CURVE('',#3154,#3156,#1963,.T.);
#3812=EDGE_CURVE('',#3157,#3156,#1964,.T.);
#3813=EDGE_CURVE('',#3155,#3157,#1965,.T.);
#3814=EDGE_CURVE('',#3158,#3159,#1966,.T.);
#3815=EDGE_CURVE('',#3160,#3158,#1967,.T.);
#3816=EDGE_CURVE('',#3161,#3160,#1968,.T.);
#3817=EDGE_CURVE('',#3161,#3159,#1969,.T.);
#3818=EDGE_CURVE('',#3159,#3154,#2743,.T.);
#3819=EDGE_CURVE('',#3156,#3161,#2744,.T.);
#3820=EDGE_CURVE('',#3160,#3158,#2745,.T.);
#3821=EDGE_CURVE('',#3162,#3157,#2746,.T.);
#3822=EDGE_CURVE('',#3155,#3162,#2747,.T.);
#3823=EDGE_CURVE('',#3163,#3163,#2748,.T.);
#3824=EDGE_CURVE('',#3164,#3164,#2749,.T.);
#3825=EDGE_CURVE('',#3163,#3162,#1970,.T.);
#3826=EDGE_CURVE('',#3165,#3165,#2750,.T.);
#3827=EDGE_CURVE('',#3165,#3164,#1971,.T.);
#3828=EDGE_CURVE('',#3166,#3167,#1972,.T.);
#3829=EDGE_CURVE('',#3166,#3168,#1973,.T.);
#3830=EDGE_CURVE('',#3169,#3168,#1974,.T.);
#3831=EDGE_CURVE('',#3167,#3169,#1975,.T.);
#3832=EDGE_CURVE('',#3170,#3171,#1976,.T.);
#3833=EDGE_CURVE('',#3172,#3170,#1977,.T.);
#3834=EDGE_CURVE('',#3173,#3172,#1978,.T.);
#3835=EDGE_CURVE('',#3173,#3171,#1979,.T.);
#3836=EDGE_CURVE('',#3171,#3166,#2751,.T.);
#3837=EDGE_CURVE('',#3168,#3173,#2752,.T.);
#3838=EDGE_CURVE('',#3172,#3170,#2753,.T.);
#3839=EDGE_CURVE('',#3174,#3169,#2754,.T.);
#3840=EDGE_CURVE('',#3167,#3174,#2755,.T.);
#3841=EDGE_CURVE('',#3175,#3175,#2756,.T.);
#3842=EDGE_CURVE('',#3176,#3176,#2757,.T.);
#3843=EDGE_CURVE('',#3175,#3174,#1980,.T.);
#3844=EDGE_CURVE('',#3177,#3177,#2758,.T.);
#3845=EDGE_CURVE('',#3177,#3176,#1981,.T.);
#3846=EDGE_CURVE('',#3178,#3179,#1982,.T.);
#3847=EDGE_CURVE('',#3178,#3180,#1983,.T.);
#3848=EDGE_CURVE('',#3181,#3180,#1984,.T.);
#3849=EDGE_CURVE('',#3179,#3181,#1985,.T.);
#3850=EDGE_CURVE('',#3182,#3183,#1986,.T.);
#3851=EDGE_CURVE('',#3184,#3182,#1987,.T.);
#3852=EDGE_CURVE('',#3185,#3184,#1988,.T.);
#3853=EDGE_CURVE('',#3185,#3183,#1989,.T.);
#3854=EDGE_CURVE('',#3183,#3178,#2759,.T.);
#3855=EDGE_CURVE('',#3180,#3185,#2760,.T.);
#3856=EDGE_CURVE('',#3184,#3182,#2761,.T.);
#3857=EDGE_CURVE('',#3186,#3181,#2762,.T.);
#3858=EDGE_CURVE('',#3179,#3186,#2763,.T.);
#3859=EDGE_CURVE('',#3187,#3187,#2764,.T.);
#3860=EDGE_CURVE('',#3188,#3188,#2765,.T.);
#3861=EDGE_CURVE('',#3187,#3186,#1990,.T.);
#3862=EDGE_CURVE('',#3189,#3189,#2766,.T.);
#3863=EDGE_CURVE('',#3189,#3188,#1991,.T.);
#3864=EDGE_CURVE('',#3190,#3190,#2767,.T.);
#3865=EDGE_CURVE('',#3190,#3191,#1992,.T.);
#3866=EDGE_CURVE('',#3191,#3191,#2768,.T.);
#3867=EDGE_CURVE('',#3192,#3192,#2769,.T.);
#3868=EDGE_CURVE('',#3192,#3193,#1993,.T.);
#3869=EDGE_CURVE('',#3193,#3193,#2770,.T.);
#3870=EDGE_CURVE('',#3194,#3194,#2771,.T.);
#3871=EDGE_CURVE('',#3194,#3195,#1994,.T.);
#3872=EDGE_CURVE('',#3195,#3195,#2772,.T.);
#3873=EDGE_CURVE('',#3196,#3196,#2773,.T.);
#3874=EDGE_CURVE('',#3196,#3197,#1995,.T.);
#3875=EDGE_CURVE('',#3197,#3197,#2774,.T.);
#3876=EDGE_CURVE('',#3198,#3198,#2775,.T.);
#3877=EDGE_CURVE('',#3198,#3199,#1996,.T.);
#3878=EDGE_CURVE('',#3199,#3199,#2776,.T.);
#3879=EDGE_CURVE('',#3200,#3200,#2777,.T.);
#3880=EDGE_CURVE('',#3200,#3201,#1997,.T.);
#3881=EDGE_CURVE('',#3201,#3201,#2778,.T.);
#3882=EDGE_CURVE('',#3202,#3202,#2779,.T.);
#3883=EDGE_CURVE('',#3202,#3203,#1998,.T.);
#3884=EDGE_CURVE('',#3203,#3203,#2780,.T.);
#3885=EDGE_CURVE('',#3204,#3204,#2781,.T.);
#3886=EDGE_CURVE('',#3204,#3205,#1999,.T.);
#3887=EDGE_CURVE('',#3205,#3205,#2782,.T.);
#3888=EDGE_CURVE('',#3206,#3206,#2783,.T.);
#3889=EDGE_CURVE('',#3206,#3207,#2000,.T.);
#3890=EDGE_CURVE('',#3207,#3207,#2784,.T.);
#3891=EDGE_CURVE('',#3208,#3208,#2785,.T.);
#3892=EDGE_CURVE('',#3208,#3209,#2001,.T.);
#3893=EDGE_CURVE('',#3209,#3209,#2786,.T.);
#3894=EDGE_CURVE('',#3210,#3210,#2787,.T.);
#3895=EDGE_CURVE('',#3210,#3211,#2002,.T.);
#3896=EDGE_CURVE('',#3211,#3211,#2788,.T.);
#3897=EDGE_CURVE('',#3212,#3212,#2789,.T.);
#3898=EDGE_CURVE('',#3212,#3213,#2003,.T.);
#3899=EDGE_CURVE('',#3213,#3213,#2790,.T.);
#3900=EDGE_CURVE('',#3214,#3214,#2791,.T.);
#3901=EDGE_CURVE('',#3214,#3215,#2004,.T.);
#3902=EDGE_CURVE('',#3215,#3215,#2792,.T.);
#3903=EDGE_CURVE('',#3216,#3216,#2793,.T.);
#3904=EDGE_CURVE('',#3217,#3217,#2794,.T.);
#3905=EDGE_CURVE('',#3218,#3218,#2795,.T.);
#3906=EDGE_CURVE('',#3218,#3216,#2005,.T.);
#3907=EDGE_CURVE('',#3217,#3219,#2006,.T.);
#3908=EDGE_CURVE('',#3219,#3219,#2796,.T.);
#3909=EDGE_CURVE('',#3220,#3221,#2007,.T.);
#3910=EDGE_CURVE('',#3221,#3222,#2008,.T.);
#3911=EDGE_CURVE('',#3223,#3222,#2009,.T.);
#3912=EDGE_CURVE('',#3220,#3223,#2010,.T.);
#3913=EDGE_CURVE('',#3224,#3220,#2011,.T.);
#3914=EDGE_CURVE('',#3225,#3223,#2012,.T.);
#3915=EDGE_CURVE('',#3224,#3225,#2013,.T.);
#3916=EDGE_CURVE('',#3226,#3224,#2014,.T.);
#3917=EDGE_CURVE('',#3227,#3225,#2015,.T.);
#3918=EDGE_CURVE('',#3226,#3227,#2016,.T.);
#3919=EDGE_CURVE('',#3221,#3226,#2017,.T.);
#3920=EDGE_CURVE('',#3222,#3227,#2018,.T.);
#3921=EDGE_CURVE('',#3228,#3229,#2019,.T.);
#3922=EDGE_CURVE('',#3229,#3230,#2020,.T.);
#3923=EDGE_CURVE('',#3231,#3230,#2021,.T.);
#3924=EDGE_CURVE('',#3228,#3231,#2022,.T.);
#3925=EDGE_CURVE('',#3232,#3228,#2023,.T.);
#3926=EDGE_CURVE('',#3233,#3231,#2024,.T.);
#3927=EDGE_CURVE('',#3232,#3233,#2025,.T.);
#3928=EDGE_CURVE('',#3234,#3232,#2026,.T.);
#3929=EDGE_CURVE('',#3235,#3233,#2027,.T.);
#3930=EDGE_CURVE('',#3234,#3235,#2028,.T.);
#3931=EDGE_CURVE('',#3229,#3234,#2029,.T.);
#3932=EDGE_CURVE('',#3230,#3235,#2030,.T.);
#3933=EDGE_CURVE('',#3236,#3237,#2031,.T.);
#3934=EDGE_CURVE('',#3237,#3238,#2032,.T.);
#3935=EDGE_CURVE('',#3238,#3239,#2033,.T.);
#3936=EDGE_CURVE('',#3236,#3239,#2034,.T.);
#3937=EDGE_CURVE('',#3237,#3240,#2035,.T.);
#3938=EDGE_CURVE('',#3240,#3241,#2036,.T.);
#3939=EDGE_CURVE('',#3241,#3238,#2037,.T.);
#3940=EDGE_CURVE('',#3240,#3242,#2038,.T.);
#3941=EDGE_CURVE('',#3242,#3243,#2039,.T.);
#3942=EDGE_CURVE('',#3243,#3241,#2040,.T.);
#3943=EDGE_CURVE('',#3242,#3244,#2041,.T.);
#3944=EDGE_CURVE('',#3244,#3245,#2042,.T.);
#3945=EDGE_CURVE('',#3245,#3243,#2043,.T.);
#3946=EDGE_CURVE('',#3244,#3246,#2044,.T.);
#3947=EDGE_CURVE('',#3246,#3247,#2045,.T.);
#3948=EDGE_CURVE('',#3247,#3245,#2046,.T.);
#3949=EDGE_CURVE('',#3246,#3236,#2047,.T.);
#3950=EDGE_CURVE('',#3239,#3247,#2048,.T.);
#3951=EDGE_CURVE('',#3248,#3248,#2797,.T.);
#3952=EDGE_CURVE('',#3249,#3249,#2798,.T.);
#3953=EDGE_CURVE('',#3250,#3250,#2799,.T.);
#3954=EDGE_CURVE('',#3250,#3249,#2049,.T.);
#3955=EDGE_CURVE('',#3251,#3251,#2800,.T.);
#3956=EDGE_CURVE('',#3251,#3250,#2050,.T.);
#3957=EDGE_CURVE('',#3252,#3252,#2801,.T.);
#3958=EDGE_CURVE('',#3252,#3251,#2051,.T.);
#3959=EDGE_CURVE('',#3253,#3253,#2802,.T.);
#3960=EDGE_CURVE('',#3254,#3254,#2803,.F.);
#3961=EDGE_CURVE('',#3254,#3253,#2052,.T.);
#3962=EDGE_CURVE('',#3248,#3254,#2053,.T.);
#3963=EDGE_CURVE('',#3255,#3255,#2804,.T.);
#3964=EDGE_CURVE('',#3255,#3256,#2054,.T.);
#3965=EDGE_CURVE('',#3256,#3256,#2805,.T.);
#3966=EDGE_CURVE('',#3257,#3257,#2806,.T.);
#3967=EDGE_CURVE('',#3258,#3259,#2055,.T.);
#3968=EDGE_CURVE('',#3259,#3260,#2056,.T.);
#3969=EDGE_CURVE('',#3260,#3261,#2057,.T.);
#3970=EDGE_CURVE('',#3261,#3262,#2058,.T.);
#3971=EDGE_CURVE('',#3262,#3263,#2059,.T.);
#3972=EDGE_CURVE('',#3263,#3258,#2060,.T.);
#3973=EDGE_CURVE('',#3264,#3264,#2807,.T.);
#3974=EDGE_CURVE('',#3265,#3266,#2061,.T.);
#3975=EDGE_CURVE('',#3267,#3265,#2062,.T.);
#3976=EDGE_CURVE('',#3268,#3267,#2063,.T.);
#3977=EDGE_CURVE('',#3269,#3268,#2064,.T.);
#3978=EDGE_CURVE('',#3270,#3269,#2065,.T.);
#3979=EDGE_CURVE('',#3266,#3270,#2066,.T.);
#3980=EDGE_CURVE('',#3271,#3271,#2808,.T.);
#3981=EDGE_CURVE('',#3265,#3258,#2067,.T.);
#3982=EDGE_CURVE('',#3267,#3263,#2068,.T.);
#3983=EDGE_CURVE('',#3268,#3262,#2069,.T.);
#3984=EDGE_CURVE('',#3269,#3261,#2070,.T.);
#3985=EDGE_CURVE('',#3270,#3260,#2071,.T.);
#3986=EDGE_CURVE('',#3266,#3259,#2072,.T.);
#3987=EDGE_CURVE('',#3272,#3272,#2809,.T.);
#3988=EDGE_CURVE('',#3272,#3273,#2073,.T.);
#3989=EDGE_CURVE('',#3273,#3273,#2810,.T.);
#3990=EDGE_CURVE('',#3274,#3274,#2811,.T.);
#3991=EDGE_CURVE('',#3264,#3274,#2074,.T.);
#3992=EDGE_CURVE('',#3275,#3275,#2812,.T.);
#3993=EDGE_CURVE('',#3275,#3271,#2075,.T.);
#3994=EDGE_CURVE('',#3276,#3276,#2813,.T.);
#3995=EDGE_CURVE('',#3276,#3257,#2076,.T.);
#3996=EDGE_CURVE('',#3277,#3277,#2814,.T.);
#3997=EDGE_CURVE('',#3278,#3278,#2815,.T.);
#3998=EDGE_CURVE('',#3279,#3279,#2816,.T.);
#3999=EDGE_CURVE('',#3279,#3277,#2077,.T.);
#4000=EDGE_CURVE('',#3280,#3280,#2817,.T.);
#4001=EDGE_CURVE('',#3281,#3281,#2818,.T.);
#4002=EDGE_CURVE('',#3281,#3280,#2078,.T.);
#4003=EDGE_CURVE('',#3282,#3282,#2819,.T.);
#4004=EDGE_CURVE('',#3282,#3278,#2079,.T.);
#4005=EDGE_CURVE('',#3283,#3284,#2080,.T.);
#4006=EDGE_CURVE('',#3284,#3285,#2081,.T.);
#4007=EDGE_CURVE('',#3285,#3286,#2082,.T.);
#4008=EDGE_CURVE('',#3286,#3287,#2083,.T.);
#4009=EDGE_CURVE('',#3287,#3288,#2084,.T.);
#4010=EDGE_CURVE('',#3288,#3283,#2085,.T.);
#4011=EDGE_CURVE('',#3289,#3289,#2820,.T.);
#4012=EDGE_CURVE('',#3290,#3291,#2086,.T.);
#4013=EDGE_CURVE('',#3291,#3292,#2087,.T.);
#4014=EDGE_CURVE('',#3292,#3293,#2088,.T.);
#4015=EDGE_CURVE('',#3293,#3294,#2089,.T.);
#4016=EDGE_CURVE('',#3294,#3295,#2090,.T.);
#4017=EDGE_CURVE('',#3295,#3290,#2091,.T.);
#4018=EDGE_CURVE('',#3296,#3296,#2821,.T.);
#4019=EDGE_CURVE('',#3290,#3284,#2092,.T.);
#4020=EDGE_CURVE('',#3285,#3295,#2093,.T.);
#4021=EDGE_CURVE('',#3286,#3294,#2094,.T.);
#4022=EDGE_CURVE('',#3287,#3293,#2095,.T.);
#4023=EDGE_CURVE('',#3288,#3292,#2096,.T.);
#4024=EDGE_CURVE('',#3283,#3291,#2097,.T.);
#4025=EDGE_CURVE('',#3296,#3297,#2098,.T.);
#4026=EDGE_CURVE('',#3297,#3297,#2822,.T.);
#4027=EDGE_CURVE('',#3298,#3298,#2823,.T.);
#4028=EDGE_CURVE('',#3299,#3299,#2824,.T.);
#4029=EDGE_CURVE('',#3297,#3298,#2099,.T.);
#4030=EDGE_CURVE('',#3300,#3300,#2825,.T.);
#4031=EDGE_CURVE('',#3300,#3289,#2100,.T.);
#4032=EDGE_CURVE('',#3301,#3301,#2826,.T.);
#4033=EDGE_CURVE('',#3301,#3300,#2101,.T.);
#4034=EDGE_CURVE('',#3302,#3302,#2827,.T.);
#4035=EDGE_CURVE('',#3302,#3299,#2102,.T.);
#4036=EDGE_CURVE('',#3303,#3303,#2828,.T.);
#4037=EDGE_CURVE('',#3304,#3304,#2829,.T.);
#4038=EDGE_CURVE('',#3304,#3303,#2103,.T.);
#4039=EDGE_CURVE('',#3305,#3305,#2830,.T.);
#4040=EDGE_CURVE('',#3305,#3304,#2104,.T.);
#4041=EDGE_CURVE('',#3306,#3306,#2831,.T.);
#4042=EDGE_CURVE('',#3306,#3305,#2105,.T.);
#4043=EDGE_CURVE('',#3307,#3307,#2832,.T.);
#4044=EDGE_CURVE('',#3308,#3308,#2833,.F.);
#4045=EDGE_CURVE('',#3308,#3307,#2106,.T.);
#4046=EDGE_CURVE('',#3309,#3309,#2834,.F.);
#4047=EDGE_CURVE('',#3309,#3308,#2107,.T.);
#4048=EDGE_CURVE('',#3310,#3310,#2835,.T.);
#4049=EDGE_CURVE('',#3310,#3309,#2108,.T.);
#4050=EDGE_CURVE('',#3311,#3312,#2109,.T.);
#4051=EDGE_CURVE('',#3312,#3313,#2110,.T.);
#4052=EDGE_CURVE('',#3313,#3314,#2111,.T.);
#4053=EDGE_CURVE('',#3311,#3314,#2112,.T.);
#4054=EDGE_CURVE('',#3312,#3315,#2113,.T.);
#4055=EDGE_CURVE('',#3315,#3316,#2114,.T.);
#4056=EDGE_CURVE('',#3316,#3313,#2115,.T.);
#4057=EDGE_CURVE('',#3315,#3317,#2116,.T.);
#4058=EDGE_CURVE('',#3317,#3318,#2117,.T.);
#4059=EDGE_CURVE('',#3318,#3316,#2118,.T.);
#4060=EDGE_CURVE('',#3317,#3319,#2119,.T.);
#4061=EDGE_CURVE('',#3319,#3320,#2120,.T.);
#4062=EDGE_CURVE('',#3320,#3318,#2121,.T.);
#4063=EDGE_CURVE('',#3319,#3321,#2122,.T.);
#4064=EDGE_CURVE('',#3321,#3322,#2123,.T.);
#4065=EDGE_CURVE('',#3322,#3320,#2124,.T.);
#4066=EDGE_CURVE('',#3321,#3311,#2125,.T.);
#4067=EDGE_CURVE('',#3314,#3322,#2126,.T.);
#4068=ORIENTED_EDGE('',*,*,#3323,.F.);
#4069=ORIENTED_EDGE('',*,*,#3324,.T.);
#4070=ORIENTED_EDGE('',*,*,#3325,.F.);
#4071=ORIENTED_EDGE('',*,*,#3324,.F.);
#4072=ORIENTED_EDGE('',*,*,#3326,.F.);
#4073=ORIENTED_EDGE('',*,*,#3327,.T.);
#4074=ORIENTED_EDGE('',*,*,#3328,.F.);
#4075=ORIENTED_EDGE('',*,*,#3327,.F.);
#4076=ORIENTED_EDGE('',*,*,#3329,.F.);
#4077=ORIENTED_EDGE('',*,*,#3330,.T.);
#4078=ORIENTED_EDGE('',*,*,#3331,.F.);
#4079=ORIENTED_EDGE('',*,*,#3330,.F.);
#4080=ORIENTED_EDGE('',*,*,#3332,.F.);
#4081=ORIENTED_EDGE('',*,*,#3333,.T.);
#4082=ORIENTED_EDGE('',*,*,#3334,.F.);
#4083=ORIENTED_EDGE('',*,*,#3333,.F.);
#4084=ORIENTED_EDGE('',*,*,#3335,.T.);
#4085=ORIENTED_EDGE('',*,*,#3336,.T.);
#4086=ORIENTED_EDGE('',*,*,#3337,.F.);
#4087=ORIENTED_EDGE('',*,*,#3338,.F.);
#4088=ORIENTED_EDGE('',*,*,#3339,.T.);
#4089=ORIENTED_EDGE('',*,*,#3338,.T.);
#4090=ORIENTED_EDGE('',*,*,#3340,.F.);
#4091=ORIENTED_EDGE('',*,*,#3341,.F.);
#4092=ORIENTED_EDGE('',*,*,#3342,.T.);
#4093=ORIENTED_EDGE('',*,*,#3341,.T.);
#4094=ORIENTED_EDGE('',*,*,#3343,.F.);
#4095=ORIENTED_EDGE('',*,*,#3344,.F.);
#4096=ORIENTED_EDGE('',*,*,#3345,.T.);
#4097=ORIENTED_EDGE('',*,*,#3344,.T.);
#4098=ORIENTED_EDGE('',*,*,#3346,.F.);
#4099=ORIENTED_EDGE('',*,*,#3336,.F.);
#4100=ORIENTED_EDGE('',*,*,#3346,.T.);
#4101=ORIENTED_EDGE('',*,*,#3343,.T.);
#4102=ORIENTED_EDGE('',*,*,#3340,.T.);
#4103=ORIENTED_EDGE('',*,*,#3337,.T.);
#4104=ORIENTED_EDGE('',*,*,#3325,.T.);
#4105=ORIENTED_EDGE('',*,*,#3328,.T.);
#4106=ORIENTED_EDGE('',*,*,#3331,.T.);
#4107=ORIENTED_EDGE('',*,*,#3334,.T.);
#4108=ORIENTED_EDGE('',*,*,#3345,.F.);
#4109=ORIENTED_EDGE('',*,*,#3335,.F.);
#4110=ORIENTED_EDGE('',*,*,#3339,.F.);
#4111=ORIENTED_EDGE('',*,*,#3342,.F.);
#4112=ORIENTED_EDGE('',*,*,#3323,.T.);
#4113=ORIENTED_EDGE('',*,*,#3326,.T.);
#4114=ORIENTED_EDGE('',*,*,#3329,.T.);
#4115=ORIENTED_EDGE('',*,*,#3332,.T.);
#4116=ORIENTED_EDGE('',*,*,#3347,.F.);
#4117=ORIENTED_EDGE('',*,*,#3348,.T.);
#4118=ORIENTED_EDGE('',*,*,#3349,.F.);
#4119=ORIENTED_EDGE('',*,*,#3348,.F.);
#4120=ORIENTED_EDGE('',*,*,#3347,.T.);
#4121=ORIENTED_EDGE('',*,*,#3350,.F.);
#4122=ORIENTED_EDGE('',*,*,#3351,.T.);
#4123=ORIENTED_EDGE('',*,*,#3352,.F.);
#4124=ORIENTED_EDGE('',*,*,#3351,.F.);
#4125=ORIENTED_EDGE('',*,*,#3350,.T.);
#4126=ORIENTED_EDGE('',*,*,#3353,.F.);
#4127=ORIENTED_EDGE('',*,*,#3354,.F.);
#4128=ORIENTED_EDGE('',*,*,#3355,.T.);
#4129=ORIENTED_EDGE('',*,*,#3356,.F.);
#4130=ORIENTED_EDGE('',*,*,#3355,.F.);
#4131=ORIENTED_EDGE('',*,*,#3354,.T.);
#4132=ORIENTED_EDGE('',*,*,#3357,.F.);
#4133=ORIENTED_EDGE('',*,*,#3358,.F.);
#4134=ORIENTED_EDGE('',*,*,#3359,.T.);
#4135=ORIENTED_EDGE('',*,*,#3353,.T.);
#4136=ORIENTED_EDGE('',*,*,#3359,.F.);
#4137=ORIENTED_EDGE('',*,*,#3360,.F.);
#4138=ORIENTED_EDGE('',*,*,#3361,.T.);
#4139=ORIENTED_EDGE('',*,*,#3357,.T.);
#4140=ORIENTED_EDGE('',*,*,#3361,.F.);
#4141=ORIENTED_EDGE('',*,*,#3362,.T.);
#4142=ORIENTED_EDGE('',*,*,#3363,.T.);
#4143=ORIENTED_EDGE('',*,*,#3364,.F.);
#4144=ORIENTED_EDGE('',*,*,#3365,.F.);
#4145=ORIENTED_EDGE('',*,*,#3366,.T.);
#4146=ORIENTED_EDGE('',*,*,#3365,.T.);
#4147=ORIENTED_EDGE('',*,*,#3367,.F.);
#4148=ORIENTED_EDGE('',*,*,#3368,.F.);
#4149=ORIENTED_EDGE('',*,*,#3369,.T.);
#4150=ORIENTED_EDGE('',*,*,#3368,.T.);
#4151=ORIENTED_EDGE('',*,*,#3370,.F.);
#4152=ORIENTED_EDGE('',*,*,#3371,.F.);
#4153=ORIENTED_EDGE('',*,*,#3372,.T.);
#4154=ORIENTED_EDGE('',*,*,#3371,.T.);
#4155=ORIENTED_EDGE('',*,*,#3373,.F.);
#4156=ORIENTED_EDGE('',*,*,#3363,.F.);
#4157=ORIENTED_EDGE('',*,*,#3373,.T.);
#4158=ORIENTED_EDGE('',*,*,#3370,.T.);
#4159=ORIENTED_EDGE('',*,*,#3367,.T.);
#4160=ORIENTED_EDGE('',*,*,#3364,.T.);
#4161=ORIENTED_EDGE('',*,*,#3349,.T.);
#4162=ORIENTED_EDGE('',*,*,#3352,.T.);
#4163=ORIENTED_EDGE('',*,*,#3356,.T.);
#4164=ORIENTED_EDGE('',*,*,#3372,.F.);
#4165=ORIENTED_EDGE('',*,*,#3362,.F.);
#4166=ORIENTED_EDGE('',*,*,#3366,.F.);
#4167=ORIENTED_EDGE('',*,*,#3369,.F.);
#4168=ORIENTED_EDGE('',*,*,#3358,.T.);
#4169=ORIENTED_EDGE('',*,*,#3360,.T.);
#4170=ORIENTED_EDGE('',*,*,#3374,.F.);
#4171=ORIENTED_EDGE('',*,*,#3375,.T.);
#4172=ORIENTED_EDGE('',*,*,#3376,.F.);
#4173=ORIENTED_EDGE('',*,*,#3375,.F.);
#4174=ORIENTED_EDGE('',*,*,#3374,.T.);
#4175=ORIENTED_EDGE('',*,*,#3377,.F.);
#4176=ORIENTED_EDGE('',*,*,#3378,.T.);
#4177=ORIENTED_EDGE('',*,*,#3379,.F.);
#4178=ORIENTED_EDGE('',*,*,#3378,.F.);
#4179=ORIENTED_EDGE('',*,*,#3377,.T.);
#4180=ORIENTED_EDGE('',*,*,#3380,.F.);
#4181=ORIENTED_EDGE('',*,*,#3381,.F.);
#4182=ORIENTED_EDGE('',*,*,#3382,.T.);
#4183=ORIENTED_EDGE('',*,*,#3383,.F.);
#4184=ORIENTED_EDGE('',*,*,#3382,.F.);
#4185=ORIENTED_EDGE('',*,*,#3381,.T.);
#4186=ORIENTED_EDGE('',*,*,#3384,.F.);
#4187=ORIENTED_EDGE('',*,*,#3385,.F.);
#4188=ORIENTED_EDGE('',*,*,#3386,.T.);
#4189=ORIENTED_EDGE('',*,*,#3380,.T.);
#4190=ORIENTED_EDGE('',*,*,#3386,.F.);
#4191=ORIENTED_EDGE('',*,*,#3387,.F.);
#4192=ORIENTED_EDGE('',*,*,#3388,.T.);
#4193=ORIENTED_EDGE('',*,*,#3384,.T.);
#4194=ORIENTED_EDGE('',*,*,#3388,.F.);
#4195=ORIENTED_EDGE('',*,*,#3389,.T.);
#4196=ORIENTED_EDGE('',*,*,#3390,.T.);
#4197=ORIENTED_EDGE('',*,*,#3391,.F.);
#4198=ORIENTED_EDGE('',*,*,#3392,.F.);
#4199=ORIENTED_EDGE('',*,*,#3393,.T.);
#4200=ORIENTED_EDGE('',*,*,#3392,.T.);
#4201=ORIENTED_EDGE('',*,*,#3394,.F.);
#4202=ORIENTED_EDGE('',*,*,#3395,.F.);
#4203=ORIENTED_EDGE('',*,*,#3396,.T.);
#4204=ORIENTED_EDGE('',*,*,#3395,.T.);
#4205=ORIENTED_EDGE('',*,*,#3397,.F.);
#4206=ORIENTED_EDGE('',*,*,#3398,.F.);
#4207=ORIENTED_EDGE('',*,*,#3399,.T.);
#4208=ORIENTED_EDGE('',*,*,#3398,.T.);
#4209=ORIENTED_EDGE('',*,*,#3400,.F.);
#4210=ORIENTED_EDGE('',*,*,#3390,.F.);
#4211=ORIENTED_EDGE('',*,*,#3400,.T.);
#4212=ORIENTED_EDGE('',*,*,#3397,.T.);
#4213=ORIENTED_EDGE('',*,*,#3394,.T.);
#4214=ORIENTED_EDGE('',*,*,#3391,.T.);
#4215=ORIENTED_EDGE('',*,*,#3376,.T.);
#4216=ORIENTED_EDGE('',*,*,#3379,.T.);
#4217=ORIENTED_EDGE('',*,*,#3383,.T.);
#4218=ORIENTED_EDGE('',*,*,#3399,.F.);
#4219=ORIENTED_EDGE('',*,*,#3389,.F.);
#4220=ORIENTED_EDGE('',*,*,#3393,.F.);
#4221=ORIENTED_EDGE('',*,*,#3396,.F.);
#4222=ORIENTED_EDGE('',*,*,#3385,.T.);
#4223=ORIENTED_EDGE('',*,*,#3387,.T.);
#4224=ORIENTED_EDGE('',*,*,#3401,.F.);
#4225=ORIENTED_EDGE('',*,*,#3402,.T.);
#4226=ORIENTED_EDGE('',*,*,#3403,.F.);
#4227=ORIENTED_EDGE('',*,*,#3404,.T.);
#4228=ORIENTED_EDGE('',*,*,#3405,.F.);
#4229=ORIENTED_EDGE('',*,*,#3406,.F.);
#4230=ORIENTED_EDGE('',*,*,#3407,.F.);
#4231=ORIENTED_EDGE('',*,*,#3402,.F.);
#4232=ORIENTED_EDGE('',*,*,#3408,.F.);
#4233=ORIENTED_EDGE('',*,*,#3409,.F.);
#4234=ORIENTED_EDGE('',*,*,#3410,.F.);
#4235=ORIENTED_EDGE('',*,*,#3411,.T.);
#4236=ORIENTED_EDGE('',*,*,#3412,.F.);
#4237=ORIENTED_EDGE('',*,*,#3413,.F.);
#4238=ORIENTED_EDGE('',*,*,#3406,.T.);
#4239=ORIENTED_EDGE('',*,*,#3414,.F.);
#4240=ORIENTED_EDGE('',*,*,#3415,.F.);
#4241=ORIENTED_EDGE('',*,*,#3416,.T.);
#4242=ORIENTED_EDGE('',*,*,#3417,.F.);
#4243=ORIENTED_EDGE('',*,*,#3411,.F.);
#4244=ORIENTED_EDGE('',*,*,#3418,.F.);
#4245=ORIENTED_EDGE('',*,*,#3419,.F.);
#4246=ORIENTED_EDGE('',*,*,#3420,.F.);
#4247=ORIENTED_EDGE('',*,*,#3404,.F.);
#4248=ORIENTED_EDGE('',*,*,#3421,.F.);
#4249=ORIENTED_EDGE('',*,*,#3422,.F.);
#4250=ORIENTED_EDGE('',*,*,#3423,.F.);
#4251=ORIENTED_EDGE('',*,*,#3424,.F.);
#4252=ORIENTED_EDGE('',*,*,#3416,.F.);
#4253=ORIENTED_EDGE('',*,*,#3425,.F.);
#4254=ORIENTED_EDGE('',*,*,#3422,.T.);
#4255=ORIENTED_EDGE('',*,*,#3408,.T.);
#4256=ORIENTED_EDGE('',*,*,#3426,.T.);
#4257=ORIENTED_EDGE('',*,*,#3401,.T.);
#4258=ORIENTED_EDGE('',*,*,#3427,.T.);
#4259=ORIENTED_EDGE('',*,*,#3409,.T.);
#4260=ORIENTED_EDGE('',*,*,#3426,.F.);
#4261=ORIENTED_EDGE('',*,*,#3420,.T.);
#4262=ORIENTED_EDGE('',*,*,#3425,.T.);
#4263=ORIENTED_EDGE('',*,*,#3421,.T.);
#4264=ORIENTED_EDGE('',*,*,#3428,.T.);
#4265=ORIENTED_EDGE('',*,*,#3429,.F.);
#4266=ORIENTED_EDGE('',*,*,#3428,.F.);
#4267=ORIENTED_EDGE('',*,*,#3410,.T.);
#4268=ORIENTED_EDGE('',*,*,#3419,.T.);
#4269=ORIENTED_EDGE('',*,*,#3403,.T.);
#4270=ORIENTED_EDGE('',*,*,#3427,.F.);
#4271=ORIENTED_EDGE('',*,*,#3418,.T.);
#4272=ORIENTED_EDGE('',*,*,#3423,.T.);
#4273=ORIENTED_EDGE('',*,*,#3430,.F.);
#4274=ORIENTED_EDGE('',*,*,#3407,.T.);
#4275=ORIENTED_EDGE('',*,*,#3430,.T.);
#4276=ORIENTED_EDGE('',*,*,#3431,.F.);
#4277=ORIENTED_EDGE('',*,*,#3432,.T.);
#4278=ORIENTED_EDGE('',*,*,#3433,.F.);
#4279=ORIENTED_EDGE('',*,*,#3432,.F.);
#4280=ORIENTED_EDGE('',*,*,#3431,.T.);
#4281=ORIENTED_EDGE('',*,*,#3429,.T.);
#4282=ORIENTED_EDGE('',*,*,#3434,.F.);
#4283=ORIENTED_EDGE('',*,*,#3435,.F.);
#4284=ORIENTED_EDGE('',*,*,#3436,.T.);
#4285=ORIENTED_EDGE('',*,*,#3437,.F.);
#4286=ORIENTED_EDGE('',*,*,#3436,.F.);
#4287=ORIENTED_EDGE('',*,*,#3438,.F.);
#4288=ORIENTED_EDGE('',*,*,#3439,.F.);
#4289=ORIENTED_EDGE('',*,*,#3440,.T.);
#4290=ORIENTED_EDGE('',*,*,#3441,.F.);
#4291=ORIENTED_EDGE('',*,*,#3440,.F.);
#4292=ORIENTED_EDGE('',*,*,#3439,.T.);
#4293=ORIENTED_EDGE('',*,*,#3437,.T.);
#4294=ORIENTED_EDGE('',*,*,#3442,.F.);
#4295=ORIENTED_EDGE('',*,*,#3443,.T.);
#4296=ORIENTED_EDGE('',*,*,#3444,.F.);
#4297=ORIENTED_EDGE('',*,*,#3445,.F.);
#4298=ORIENTED_EDGE('',*,*,#3443,.F.);
#4299=ORIENTED_EDGE('',*,*,#3446,.F.);
#4300=ORIENTED_EDGE('',*,*,#3447,.T.);
#4301=ORIENTED_EDGE('',*,*,#3448,.T.);
#4302=ORIENTED_EDGE('',*,*,#3447,.F.);
#4303=ORIENTED_EDGE('',*,*,#3448,.F.);
#4304=ORIENTED_EDGE('',*,*,#3442,.T.);
#4305=ORIENTED_EDGE('',*,*,#3449,.F.);
#4306=ORIENTED_EDGE('',*,*,#3450,.F.);
#4307=ORIENTED_EDGE('',*,*,#3451,.T.);
#4308=ORIENTED_EDGE('',*,*,#3452,.F.);
#4309=ORIENTED_EDGE('',*,*,#3451,.F.);
#4310=ORIENTED_EDGE('',*,*,#3453,.F.);
#4311=ORIENTED_EDGE('',*,*,#3454,.F.);
#4312=ORIENTED_EDGE('',*,*,#3455,.T.);
#4313=ORIENTED_EDGE('',*,*,#3456,.F.);
#4314=ORIENTED_EDGE('',*,*,#3455,.F.);
#4315=ORIENTED_EDGE('',*,*,#3454,.T.);
#4316=ORIENTED_EDGE('',*,*,#3452,.T.);
#4317=ORIENTED_EDGE('',*,*,#3457,.F.);
#4318=ORIENTED_EDGE('',*,*,#3458,.T.);
#4319=ORIENTED_EDGE('',*,*,#3459,.F.);
#4320=ORIENTED_EDGE('',*,*,#3460,.F.);
#4321=ORIENTED_EDGE('',*,*,#3458,.F.);
#4322=ORIENTED_EDGE('',*,*,#3461,.F.);
#4323=ORIENTED_EDGE('',*,*,#3462,.T.);
#4324=ORIENTED_EDGE('',*,*,#3463,.T.);
#4325=ORIENTED_EDGE('',*,*,#3462,.F.);
#4326=ORIENTED_EDGE('',*,*,#3463,.F.);
#4327=ORIENTED_EDGE('',*,*,#3457,.T.);
#4328=ORIENTED_EDGE('',*,*,#3464,.F.);
#4329=ORIENTED_EDGE('',*,*,#3465,.F.);
#4330=ORIENTED_EDGE('',*,*,#3466,.T.);
#4331=ORIENTED_EDGE('',*,*,#3467,.F.);
#4332=ORIENTED_EDGE('',*,*,#3466,.F.);
#4333=ORIENTED_EDGE('',*,*,#3468,.F.);
#4334=ORIENTED_EDGE('',*,*,#3469,.F.);
#4335=ORIENTED_EDGE('',*,*,#3470,.T.);
#4336=ORIENTED_EDGE('',*,*,#3471,.F.);
#4337=ORIENTED_EDGE('',*,*,#3470,.F.);
#4338=ORIENTED_EDGE('',*,*,#3469,.T.);
#4339=ORIENTED_EDGE('',*,*,#3467,.T.);
#4340=ORIENTED_EDGE('',*,*,#3472,.F.);
#4341=ORIENTED_EDGE('',*,*,#3473,.T.);
#4342=ORIENTED_EDGE('',*,*,#3474,.F.);
#4343=ORIENTED_EDGE('',*,*,#3475,.F.);
#4344=ORIENTED_EDGE('',*,*,#3473,.F.);
#4345=ORIENTED_EDGE('',*,*,#3476,.F.);
#4346=ORIENTED_EDGE('',*,*,#3477,.T.);
#4347=ORIENTED_EDGE('',*,*,#3478,.T.);
#4348=ORIENTED_EDGE('',*,*,#3477,.F.);
#4349=ORIENTED_EDGE('',*,*,#3478,.F.);
#4350=ORIENTED_EDGE('',*,*,#3472,.T.);
#4351=ORIENTED_EDGE('',*,*,#3479,.F.);
#4352=ORIENTED_EDGE('',*,*,#3480,.F.);
#4353=ORIENTED_EDGE('',*,*,#3481,.T.);
#4354=ORIENTED_EDGE('',*,*,#3482,.F.);
#4355=ORIENTED_EDGE('',*,*,#3481,.F.);
#4356=ORIENTED_EDGE('',*,*,#3483,.F.);
#4357=ORIENTED_EDGE('',*,*,#3484,.F.);
#4358=ORIENTED_EDGE('',*,*,#3485,.T.);
#4359=ORIENTED_EDGE('',*,*,#3486,.F.);
#4360=ORIENTED_EDGE('',*,*,#3485,.F.);
#4361=ORIENTED_EDGE('',*,*,#3484,.T.);
#4362=ORIENTED_EDGE('',*,*,#3482,.T.);
#4363=ORIENTED_EDGE('',*,*,#3487,.F.);
#4364=ORIENTED_EDGE('',*,*,#3488,.T.);
#4365=ORIENTED_EDGE('',*,*,#3489,.F.);
#4366=ORIENTED_EDGE('',*,*,#3490,.F.);
#4367=ORIENTED_EDGE('',*,*,#3488,.F.);
#4368=ORIENTED_EDGE('',*,*,#3491,.F.);
#4369=ORIENTED_EDGE('',*,*,#3492,.T.);
#4370=ORIENTED_EDGE('',*,*,#3493,.T.);
#4371=ORIENTED_EDGE('',*,*,#3492,.F.);
#4372=ORIENTED_EDGE('',*,*,#3493,.F.);
#4373=ORIENTED_EDGE('',*,*,#3487,.T.);
#4374=ORIENTED_EDGE('',*,*,#3494,.F.);
#4375=ORIENTED_EDGE('',*,*,#3495,.T.);
#4376=ORIENTED_EDGE('',*,*,#3480,.T.);
#4377=ORIENTED_EDGE('',*,*,#3479,.T.);
#4378=ORIENTED_EDGE('',*,*,#3496,.T.);
#4379=ORIENTED_EDGE('',*,*,#3465,.T.);
#4380=ORIENTED_EDGE('',*,*,#3464,.T.);
#4381=ORIENTED_EDGE('',*,*,#3497,.T.);
#4382=ORIENTED_EDGE('',*,*,#3412,.T.);
#4383=ORIENTED_EDGE('',*,*,#3417,.T.);
#4384=ORIENTED_EDGE('',*,*,#3424,.T.);
#4385=ORIENTED_EDGE('',*,*,#3415,.T.);
#4386=ORIENTED_EDGE('',*,*,#3498,.T.);
#4387=ORIENTED_EDGE('',*,*,#3450,.T.);
#4388=ORIENTED_EDGE('',*,*,#3449,.T.);
#4389=ORIENTED_EDGE('',*,*,#3499,.T.);
#4390=ORIENTED_EDGE('',*,*,#3435,.T.);
#4391=ORIENTED_EDGE('',*,*,#3434,.T.);
#4392=ORIENTED_EDGE('',*,*,#3500,.T.);
#4393=ORIENTED_EDGE('',*,*,#3501,.F.);
#4394=ORIENTED_EDGE('',*,*,#3500,.F.);
#4395=ORIENTED_EDGE('',*,*,#3438,.T.);
#4396=ORIENTED_EDGE('',*,*,#3499,.F.);
#4397=ORIENTED_EDGE('',*,*,#3453,.T.);
#4398=ORIENTED_EDGE('',*,*,#3498,.F.);
#4399=ORIENTED_EDGE('',*,*,#3414,.T.);
#4400=ORIENTED_EDGE('',*,*,#3405,.T.);
#4401=ORIENTED_EDGE('',*,*,#3413,.T.);
#4402=ORIENTED_EDGE('',*,*,#3497,.F.);
#4403=ORIENTED_EDGE('',*,*,#3468,.T.);
#4404=ORIENTED_EDGE('',*,*,#3496,.F.);
#4405=ORIENTED_EDGE('',*,*,#3483,.T.);
#4406=ORIENTED_EDGE('',*,*,#3495,.F.);
#4407=ORIENTED_EDGE('',*,*,#3444,.T.);
#4408=ORIENTED_EDGE('',*,*,#3445,.T.);
#4409=ORIENTED_EDGE('',*,*,#3459,.T.);
#4410=ORIENTED_EDGE('',*,*,#3460,.T.);
#4411=ORIENTED_EDGE('',*,*,#3474,.T.);
#4412=ORIENTED_EDGE('',*,*,#3475,.T.);
#4413=ORIENTED_EDGE('',*,*,#3489,.T.);
#4414=ORIENTED_EDGE('',*,*,#3490,.T.);
#4415=ORIENTED_EDGE('',*,*,#3502,.F.);
#4416=ORIENTED_EDGE('',*,*,#3503,.T.);
#4417=ORIENTED_EDGE('',*,*,#3504,.F.);
#4418=ORIENTED_EDGE('',*,*,#3503,.F.);
#4419=ORIENTED_EDGE('',*,*,#3502,.T.);
#4420=ORIENTED_EDGE('',*,*,#3505,.F.);
#4421=ORIENTED_EDGE('',*,*,#3506,.F.);
#4422=ORIENTED_EDGE('',*,*,#3507,.T.);
#4423=ORIENTED_EDGE('',*,*,#3508,.F.);
#4424=ORIENTED_EDGE('',*,*,#3507,.F.);
#4425=ORIENTED_EDGE('',*,*,#3506,.T.);
#4426=ORIENTED_EDGE('',*,*,#3509,.F.);
#4427=ORIENTED_EDGE('',*,*,#3510,.F.);
#4428=ORIENTED_EDGE('',*,*,#3511,.T.);
#4429=ORIENTED_EDGE('',*,*,#3512,.F.);
#4430=ORIENTED_EDGE('',*,*,#3511,.F.);
#4431=ORIENTED_EDGE('',*,*,#3510,.T.);
#4432=ORIENTED_EDGE('',*,*,#3513,.F.);
#4433=ORIENTED_EDGE('',*,*,#3514,.F.);
#4434=ORIENTED_EDGE('',*,*,#3515,.T.);
#4435=ORIENTED_EDGE('',*,*,#3516,.F.);
#4436=ORIENTED_EDGE('',*,*,#3515,.F.);
#4437=ORIENTED_EDGE('',*,*,#3514,.T.);
#4438=ORIENTED_EDGE('',*,*,#3517,.F.);
#4439=ORIENTED_EDGE('',*,*,#3518,.F.);
#4440=ORIENTED_EDGE('',*,*,#3519,.T.);
#4441=ORIENTED_EDGE('',*,*,#3505,.T.);
#4442=ORIENTED_EDGE('',*,*,#3519,.F.);
#4443=ORIENTED_EDGE('',*,*,#3520,.F.);
#4444=ORIENTED_EDGE('',*,*,#3521,.T.);
#4445=ORIENTED_EDGE('',*,*,#3509,.T.);
#4446=ORIENTED_EDGE('',*,*,#3521,.F.);
#4447=ORIENTED_EDGE('',*,*,#3522,.F.);
#4448=ORIENTED_EDGE('',*,*,#3523,.T.);
#4449=ORIENTED_EDGE('',*,*,#3513,.T.);
#4450=ORIENTED_EDGE('',*,*,#3523,.F.);
#4451=ORIENTED_EDGE('',*,*,#3524,.F.);
#4452=ORIENTED_EDGE('',*,*,#3525,.T.);
#4453=ORIENTED_EDGE('',*,*,#3517,.T.);
#4454=ORIENTED_EDGE('',*,*,#3525,.F.);
#4455=ORIENTED_EDGE('',*,*,#3526,.T.);
#4456=ORIENTED_EDGE('',*,*,#3527,.T.);
#4457=ORIENTED_EDGE('',*,*,#3528,.F.);
#4458=ORIENTED_EDGE('',*,*,#3529,.F.);
#4459=ORIENTED_EDGE('',*,*,#3530,.T.);
#4460=ORIENTED_EDGE('',*,*,#3529,.T.);
#4461=ORIENTED_EDGE('',*,*,#3531,.F.);
#4462=ORIENTED_EDGE('',*,*,#3532,.F.);
#4463=ORIENTED_EDGE('',*,*,#3501,.T.);
#4464=ORIENTED_EDGE('',*,*,#3533,.T.);
#4465=ORIENTED_EDGE('',*,*,#3532,.T.);
#4466=ORIENTED_EDGE('',*,*,#3534,.F.);
#4467=ORIENTED_EDGE('',*,*,#3535,.F.);
#4468=ORIENTED_EDGE('',*,*,#3446,.T.);
#4469=ORIENTED_EDGE('',*,*,#3461,.T.);
#4470=ORIENTED_EDGE('',*,*,#3476,.T.);
#4471=ORIENTED_EDGE('',*,*,#3491,.T.);
#4472=ORIENTED_EDGE('',*,*,#3536,.T.);
#4473=ORIENTED_EDGE('',*,*,#3535,.T.);
#4474=ORIENTED_EDGE('',*,*,#3537,.F.);
#4475=ORIENTED_EDGE('',*,*,#3527,.F.);
#4476=ORIENTED_EDGE('',*,*,#3494,.T.);
#4477=ORIENTED_EDGE('',*,*,#3537,.T.);
#4478=ORIENTED_EDGE('',*,*,#3534,.T.);
#4479=ORIENTED_EDGE('',*,*,#3531,.T.);
#4480=ORIENTED_EDGE('',*,*,#3528,.T.);
#4481=ORIENTED_EDGE('',*,*,#3441,.T.);
#4482=ORIENTED_EDGE('',*,*,#3456,.T.);
#4483=ORIENTED_EDGE('',*,*,#3471,.T.);
#4484=ORIENTED_EDGE('',*,*,#3486,.T.);
#4485=ORIENTED_EDGE('',*,*,#3516,.T.);
#4486=ORIENTED_EDGE('',*,*,#3512,.T.);
#4487=ORIENTED_EDGE('',*,*,#3508,.T.);
#4488=ORIENTED_EDGE('',*,*,#3504,.T.);
#4489=ORIENTED_EDGE('',*,*,#3433,.T.);
#4490=ORIENTED_EDGE('',*,*,#3536,.F.);
#4491=ORIENTED_EDGE('',*,*,#3526,.F.);
#4492=ORIENTED_EDGE('',*,*,#3530,.F.);
#4493=ORIENTED_EDGE('',*,*,#3533,.F.);
#4494=ORIENTED_EDGE('',*,*,#3518,.T.);
#4495=ORIENTED_EDGE('',*,*,#3520,.T.);
#4496=ORIENTED_EDGE('',*,*,#3522,.T.);
#4497=ORIENTED_EDGE('',*,*,#3524,.T.);
#4498=ORIENTED_EDGE('',*,*,#3538,.F.);
#4499=ORIENTED_EDGE('',*,*,#3539,.T.);
#4500=ORIENTED_EDGE('',*,*,#3540,.T.);
#4501=ORIENTED_EDGE('',*,*,#3539,.F.);
#4502=ORIENTED_EDGE('',*,*,#3541,.F.);
#4503=ORIENTED_EDGE('',*,*,#3542,.T.);
#4504=ORIENTED_EDGE('',*,*,#3543,.T.);
#4505=ORIENTED_EDGE('',*,*,#3542,.F.);
#4506=ORIENTED_EDGE('',*,*,#3541,.T.);
#4507=ORIENTED_EDGE('',*,*,#3538,.T.);
#4508=ORIENTED_EDGE('',*,*,#3543,.F.);
#4509=ORIENTED_EDGE('',*,*,#3540,.F.);
#4510=ORIENTED_EDGE('',*,*,#3544,.F.);
#4511=ORIENTED_EDGE('',*,*,#3545,.T.);
#4512=ORIENTED_EDGE('',*,*,#3546,.F.);
#4513=ORIENTED_EDGE('',*,*,#3547,.T.);
#4514=ORIENTED_EDGE('',*,*,#3544,.T.);
#4515=ORIENTED_EDGE('',*,*,#3547,.F.);
#4516=ORIENTED_EDGE('',*,*,#3546,.T.);
#4517=ORIENTED_EDGE('',*,*,#3548,.F.);
#4518=ORIENTED_EDGE('',*,*,#3549,.T.);
#4519=ORIENTED_EDGE('',*,*,#3545,.F.);
#4520=ORIENTED_EDGE('',*,*,#3550,.T.);
#4521=ORIENTED_EDGE('',*,*,#3548,.T.);
#4522=ORIENTED_EDGE('',*,*,#3550,.F.);
#4523=ORIENTED_EDGE('',*,*,#3549,.F.);
#4524=ORIENTED_EDGE('',*,*,#3551,.T.);
#4525=ORIENTED_EDGE('',*,*,#3552,.T.);
#4526=ORIENTED_EDGE('',*,*,#3551,.F.);
#4527=ORIENTED_EDGE('',*,*,#3552,.F.);
#4528=ORIENTED_EDGE('',*,*,#3553,.F.);
#4529=ORIENTED_EDGE('',*,*,#3554,.T.);
#4530=ORIENTED_EDGE('',*,*,#3555,.T.);
#4531=ORIENTED_EDGE('',*,*,#3554,.F.);
#4532=ORIENTED_EDGE('',*,*,#3556,.F.);
#4533=ORIENTED_EDGE('',*,*,#3557,.T.);
#4534=ORIENTED_EDGE('',*,*,#3558,.T.);
#4535=ORIENTED_EDGE('',*,*,#3557,.F.);
#4536=ORIENTED_EDGE('',*,*,#3556,.T.);
#4537=ORIENTED_EDGE('',*,*,#3553,.T.);
#4538=ORIENTED_EDGE('',*,*,#3558,.F.);
#4539=ORIENTED_EDGE('',*,*,#3555,.F.);
#4540=ORIENTED_EDGE('',*,*,#3559,.F.);
#4541=ORIENTED_EDGE('',*,*,#3560,.T.);
#4542=ORIENTED_EDGE('',*,*,#3561,.T.);
#4543=ORIENTED_EDGE('',*,*,#3560,.F.);
#4544=ORIENTED_EDGE('',*,*,#3562,.F.);
#4545=ORIENTED_EDGE('',*,*,#3563,.T.);
#4546=ORIENTED_EDGE('',*,*,#3564,.T.);
#4547=ORIENTED_EDGE('',*,*,#3563,.F.);
#4548=ORIENTED_EDGE('',*,*,#3562,.T.);
#4549=ORIENTED_EDGE('',*,*,#3559,.T.);
#4550=ORIENTED_EDGE('',*,*,#3564,.F.);
#4551=ORIENTED_EDGE('',*,*,#3561,.F.);
#4552=ORIENTED_EDGE('',*,*,#3565,.F.);
#4553=ORIENTED_EDGE('',*,*,#3566,.T.);
#4554=ORIENTED_EDGE('',*,*,#3567,.F.);
#4555=ORIENTED_EDGE('',*,*,#3568,.T.);
#4556=ORIENTED_EDGE('',*,*,#3565,.T.);
#4557=ORIENTED_EDGE('',*,*,#3568,.F.);
#4558=ORIENTED_EDGE('',*,*,#3567,.T.);
#4559=ORIENTED_EDGE('',*,*,#3569,.F.);
#4560=ORIENTED_EDGE('',*,*,#3570,.T.);
#4561=ORIENTED_EDGE('',*,*,#3566,.F.);
#4562=ORIENTED_EDGE('',*,*,#3571,.T.);
#4563=ORIENTED_EDGE('',*,*,#3569,.T.);
#4564=ORIENTED_EDGE('',*,*,#3571,.F.);
#4565=ORIENTED_EDGE('',*,*,#3570,.F.);
#4566=ORIENTED_EDGE('',*,*,#3572,.T.);
#4567=ORIENTED_EDGE('',*,*,#3573,.T.);
#4568=ORIENTED_EDGE('',*,*,#3572,.F.);
#4569=ORIENTED_EDGE('',*,*,#3573,.F.);
#4570=ORIENTED_EDGE('',*,*,#3574,.F.);
#4571=ORIENTED_EDGE('',*,*,#3575,.T.);
#4572=ORIENTED_EDGE('',*,*,#3576,.T.);
#4573=ORIENTED_EDGE('',*,*,#3575,.F.);
#4574=ORIENTED_EDGE('',*,*,#3577,.F.);
#4575=ORIENTED_EDGE('',*,*,#3578,.T.);
#4576=ORIENTED_EDGE('',*,*,#3579,.T.);
#4577=ORIENTED_EDGE('',*,*,#3578,.F.);
#4578=ORIENTED_EDGE('',*,*,#3577,.T.);
#4579=ORIENTED_EDGE('',*,*,#3574,.T.);
#4580=ORIENTED_EDGE('',*,*,#3579,.F.);
#4581=ORIENTED_EDGE('',*,*,#3576,.F.);
#4582=ORIENTED_EDGE('',*,*,#3580,.F.);
#4583=ORIENTED_EDGE('',*,*,#3581,.T.);
#4584=ORIENTED_EDGE('',*,*,#3582,.T.);
#4585=ORIENTED_EDGE('',*,*,#3581,.F.);
#4586=ORIENTED_EDGE('',*,*,#3583,.F.);
#4587=ORIENTED_EDGE('',*,*,#3584,.T.);
#4588=ORIENTED_EDGE('',*,*,#3585,.T.);
#4589=ORIENTED_EDGE('',*,*,#3584,.F.);
#4590=ORIENTED_EDGE('',*,*,#3583,.T.);
#4591=ORIENTED_EDGE('',*,*,#3580,.T.);
#4592=ORIENTED_EDGE('',*,*,#3585,.F.);
#4593=ORIENTED_EDGE('',*,*,#3582,.F.);
#4594=ORIENTED_EDGE('',*,*,#3586,.F.);
#4595=ORIENTED_EDGE('',*,*,#3587,.T.);
#4596=ORIENTED_EDGE('',*,*,#3588,.F.);
#4597=ORIENTED_EDGE('',*,*,#3589,.T.);
#4598=ORIENTED_EDGE('',*,*,#3586,.T.);
#4599=ORIENTED_EDGE('',*,*,#3589,.F.);
#4600=ORIENTED_EDGE('',*,*,#3588,.T.);
#4601=ORIENTED_EDGE('',*,*,#3590,.F.);
#4602=ORIENTED_EDGE('',*,*,#3591,.T.);
#4603=ORIENTED_EDGE('',*,*,#3587,.F.);
#4604=ORIENTED_EDGE('',*,*,#3592,.T.);
#4605=ORIENTED_EDGE('',*,*,#3590,.T.);
#4606=ORIENTED_EDGE('',*,*,#3592,.F.);
#4607=ORIENTED_EDGE('',*,*,#3591,.F.);
#4608=ORIENTED_EDGE('',*,*,#3593,.T.);
#4609=ORIENTED_EDGE('',*,*,#3594,.T.);
#4610=ORIENTED_EDGE('',*,*,#3593,.F.);
#4611=ORIENTED_EDGE('',*,*,#3594,.F.);
#4612=ORIENTED_EDGE('',*,*,#3595,.F.);
#4613=ORIENTED_EDGE('',*,*,#3596,.T.);
#4614=ORIENTED_EDGE('',*,*,#3597,.T.);
#4615=ORIENTED_EDGE('',*,*,#3596,.F.);
#4616=ORIENTED_EDGE('',*,*,#3598,.F.);
#4617=ORIENTED_EDGE('',*,*,#3599,.T.);
#4618=ORIENTED_EDGE('',*,*,#3600,.T.);
#4619=ORIENTED_EDGE('',*,*,#3599,.F.);
#4620=ORIENTED_EDGE('',*,*,#3598,.T.);
#4621=ORIENTED_EDGE('',*,*,#3595,.T.);
#4622=ORIENTED_EDGE('',*,*,#3600,.F.);
#4623=ORIENTED_EDGE('',*,*,#3597,.F.);
#4624=ORIENTED_EDGE('',*,*,#3601,.F.);
#4625=ORIENTED_EDGE('',*,*,#3602,.T.);
#4626=ORIENTED_EDGE('',*,*,#3603,.T.);
#4627=ORIENTED_EDGE('',*,*,#3602,.F.);
#4628=ORIENTED_EDGE('',*,*,#3604,.F.);
#4629=ORIENTED_EDGE('',*,*,#3605,.T.);
#4630=ORIENTED_EDGE('',*,*,#3606,.T.);
#4631=ORIENTED_EDGE('',*,*,#3605,.F.);
#4632=ORIENTED_EDGE('',*,*,#3604,.T.);
#4633=ORIENTED_EDGE('',*,*,#3601,.T.);
#4634=ORIENTED_EDGE('',*,*,#3606,.F.);
#4635=ORIENTED_EDGE('',*,*,#3603,.F.);
#4636=ORIENTED_EDGE('',*,*,#3607,.F.);
#4637=ORIENTED_EDGE('',*,*,#3608,.T.);
#4638=ORIENTED_EDGE('',*,*,#3609,.F.);
#4639=ORIENTED_EDGE('',*,*,#3610,.T.);
#4640=ORIENTED_EDGE('',*,*,#3607,.T.);
#4641=ORIENTED_EDGE('',*,*,#3610,.F.);
#4642=ORIENTED_EDGE('',*,*,#3609,.T.);
#4643=ORIENTED_EDGE('',*,*,#3611,.F.);
#4644=ORIENTED_EDGE('',*,*,#3612,.T.);
#4645=ORIENTED_EDGE('',*,*,#3608,.F.);
#4646=ORIENTED_EDGE('',*,*,#3613,.T.);
#4647=ORIENTED_EDGE('',*,*,#3611,.T.);
#4648=ORIENTED_EDGE('',*,*,#3613,.F.);
#4649=ORIENTED_EDGE('',*,*,#3612,.F.);
#4650=ORIENTED_EDGE('',*,*,#3614,.T.);
#4651=ORIENTED_EDGE('',*,*,#3615,.T.);
#4652=ORIENTED_EDGE('',*,*,#3614,.F.);
#4653=ORIENTED_EDGE('',*,*,#3615,.F.);
#4654=ORIENTED_EDGE('',*,*,#3616,.F.);
#4655=ORIENTED_EDGE('',*,*,#3617,.T.);
#4656=ORIENTED_EDGE('',*,*,#3618,.T.);
#4657=ORIENTED_EDGE('',*,*,#3617,.F.);
#4658=ORIENTED_EDGE('',*,*,#3619,.F.);
#4659=ORIENTED_EDGE('',*,*,#3620,.T.);
#4660=ORIENTED_EDGE('',*,*,#3621,.T.);
#4661=ORIENTED_EDGE('',*,*,#3620,.F.);
#4662=ORIENTED_EDGE('',*,*,#3619,.T.);
#4663=ORIENTED_EDGE('',*,*,#3616,.T.);
#4664=ORIENTED_EDGE('',*,*,#3621,.F.);
#4665=ORIENTED_EDGE('',*,*,#3618,.F.);
#4666=ORIENTED_EDGE('',*,*,#3622,.F.);
#4667=ORIENTED_EDGE('',*,*,#3623,.T.);
#4668=ORIENTED_EDGE('',*,*,#3624,.T.);
#4669=ORIENTED_EDGE('',*,*,#3623,.F.);
#4670=ORIENTED_EDGE('',*,*,#3622,.T.);
#4671=ORIENTED_EDGE('',*,*,#3624,.F.);
#4672=ORIENTED_EDGE('',*,*,#3625,.F.);
#4673=ORIENTED_EDGE('',*,*,#3626,.T.);
#4674=ORIENTED_EDGE('',*,*,#3627,.T.);
#4675=ORIENTED_EDGE('',*,*,#3626,.F.);
#4676=ORIENTED_EDGE('',*,*,#3625,.T.);
#4677=ORIENTED_EDGE('',*,*,#3627,.F.);
#4678=ORIENTED_EDGE('',*,*,#3628,.F.);
#4679=ORIENTED_EDGE('',*,*,#3629,.T.);
#4680=ORIENTED_EDGE('',*,*,#3630,.F.);
#4681=ORIENTED_EDGE('',*,*,#3629,.F.);
#4682=ORIENTED_EDGE('',*,*,#3628,.T.);
#4683=ORIENTED_EDGE('',*,*,#3631,.F.);
#4684=ORIENTED_EDGE('',*,*,#3632,.T.);
#4685=ORIENTED_EDGE('',*,*,#3633,.F.);
#4686=ORIENTED_EDGE('',*,*,#3632,.F.);
#4687=ORIENTED_EDGE('',*,*,#3631,.T.);
#4688=ORIENTED_EDGE('',*,*,#3634,.F.);
#4689=ORIENTED_EDGE('',*,*,#3635,.T.);
#4690=ORIENTED_EDGE('',*,*,#3636,.F.);
#4691=ORIENTED_EDGE('',*,*,#3635,.F.);
#4692=ORIENTED_EDGE('',*,*,#3634,.T.);
#4693=ORIENTED_EDGE('',*,*,#3637,.F.);
#4694=ORIENTED_EDGE('',*,*,#3638,.T.);
#4695=ORIENTED_EDGE('',*,*,#3639,.F.);
#4696=ORIENTED_EDGE('',*,*,#3638,.F.);
#4697=ORIENTED_EDGE('',*,*,#3637,.T.);
#4698=ORIENTED_EDGE('',*,*,#3640,.F.);
#4699=ORIENTED_EDGE('',*,*,#3641,.T.);
#4700=ORIENTED_EDGE('',*,*,#3642,.F.);
#4701=ORIENTED_EDGE('',*,*,#3641,.F.);
#4702=ORIENTED_EDGE('',*,*,#3643,.F.);
#4703=ORIENTED_EDGE('',*,*,#3644,.T.);
#4704=ORIENTED_EDGE('',*,*,#3645,.F.);
#4705=ORIENTED_EDGE('',*,*,#3644,.F.);
#4706=ORIENTED_EDGE('',*,*,#3646,.F.);
#4707=ORIENTED_EDGE('',*,*,#3647,.T.);
#4708=ORIENTED_EDGE('',*,*,#3648,.F.);
#4709=ORIENTED_EDGE('',*,*,#3647,.F.);
#4710=ORIENTED_EDGE('',*,*,#3649,.F.);
#4711=ORIENTED_EDGE('',*,*,#3650,.T.);
#4712=ORIENTED_EDGE('',*,*,#3651,.F.);
#4713=ORIENTED_EDGE('',*,*,#3650,.F.);
#4714=ORIENTED_EDGE('',*,*,#3652,.F.);
#4715=ORIENTED_EDGE('',*,*,#3653,.F.);
#4716=ORIENTED_EDGE('',*,*,#3654,.F.);
#4717=ORIENTED_EDGE('',*,*,#3655,.T.);
#4718=ORIENTED_EDGE('',*,*,#3656,.F.);
#4719=ORIENTED_EDGE('',*,*,#3657,.F.);
#4720=ORIENTED_EDGE('',*,*,#3658,.F.);
#4721=ORIENTED_EDGE('',*,*,#3659,.F.);
#4722=ORIENTED_EDGE('',*,*,#3660,.F.);
#4723=ORIENTED_EDGE('',*,*,#3661,.T.);
#4724=ORIENTED_EDGE('',*,*,#3662,.F.);
#4725=ORIENTED_EDGE('',*,*,#3655,.F.);
#4726=ORIENTED_EDGE('',*,*,#3663,.F.);
#4727=ORIENTED_EDGE('',*,*,#3664,.F.);
#4728=ORIENTED_EDGE('',*,*,#3661,.F.);
#4729=ORIENTED_EDGE('',*,*,#3665,.F.);
#4730=ORIENTED_EDGE('',*,*,#3657,.T.);
#4731=ORIENTED_EDGE('',*,*,#3666,.F.);
#4732=ORIENTED_EDGE('',*,*,#3667,.F.);
#4733=ORIENTED_EDGE('',*,*,#3653,.T.);
#4734=ORIENTED_EDGE('',*,*,#3658,.T.);
#4735=ORIENTED_EDGE('',*,*,#3665,.T.);
#4736=ORIENTED_EDGE('',*,*,#3660,.T.);
#4737=ORIENTED_EDGE('',*,*,#3668,.T.);
#4738=ORIENTED_EDGE('',*,*,#3669,.F.);
#4739=ORIENTED_EDGE('',*,*,#3670,.F.);
#4740=ORIENTED_EDGE('',*,*,#3671,.F.);
#4741=ORIENTED_EDGE('',*,*,#3672,.T.);
#4742=ORIENTED_EDGE('',*,*,#3640,.T.);
#4743=ORIENTED_EDGE('',*,*,#3649,.T.);
#4744=ORIENTED_EDGE('',*,*,#3673,.F.);
#4745=ORIENTED_EDGE('',*,*,#3674,.T.);
#4746=ORIENTED_EDGE('',*,*,#3670,.T.);
#4747=ORIENTED_EDGE('',*,*,#3675,.F.);
#4748=ORIENTED_EDGE('',*,*,#3676,.F.);
#4749=ORIENTED_EDGE('',*,*,#3675,.T.);
#4750=ORIENTED_EDGE('',*,*,#3669,.T.);
#4751=ORIENTED_EDGE('',*,*,#3677,.T.);
#4752=ORIENTED_EDGE('',*,*,#3678,.F.);
#4753=ORIENTED_EDGE('',*,*,#3679,.F.);
#4754=ORIENTED_EDGE('',*,*,#3678,.T.);
#4755=ORIENTED_EDGE('',*,*,#3680,.T.);
#4756=ORIENTED_EDGE('',*,*,#3681,.F.);
#4757=ORIENTED_EDGE('',*,*,#3682,.F.);
#4758=ORIENTED_EDGE('',*,*,#3681,.T.);
#4759=ORIENTED_EDGE('',*,*,#3683,.T.);
#4760=ORIENTED_EDGE('',*,*,#3671,.T.);
#4761=ORIENTED_EDGE('',*,*,#3674,.F.);
#4762=ORIENTED_EDGE('',*,*,#3667,.T.);
#4763=ORIENTED_EDGE('',*,*,#3684,.F.);
#4764=ORIENTED_EDGE('',*,*,#3683,.F.);
#4765=ORIENTED_EDGE('',*,*,#3680,.F.);
#4766=ORIENTED_EDGE('',*,*,#3677,.F.);
#4767=ORIENTED_EDGE('',*,*,#3685,.F.);
#4768=ORIENTED_EDGE('',*,*,#3663,.T.);
#4769=ORIENTED_EDGE('',*,*,#3654,.T.);
#4770=ORIENTED_EDGE('',*,*,#3643,.T.);
#4771=ORIENTED_EDGE('',*,*,#3646,.T.);
#4772=ORIENTED_EDGE('',*,*,#3686,.F.);
#4773=ORIENTED_EDGE('',*,*,#3687,.T.);
#4774=ORIENTED_EDGE('',*,*,#3688,.F.);
#4775=ORIENTED_EDGE('',*,*,#3687,.F.);
#4776=ORIENTED_EDGE('',*,*,#3689,.F.);
#4777=ORIENTED_EDGE('',*,*,#3690,.T.);
#4778=ORIENTED_EDGE('',*,*,#3668,.F.);
#4779=ORIENTED_EDGE('',*,*,#3659,.T.);
#4780=ORIENTED_EDGE('',*,*,#3664,.T.);
#4781=ORIENTED_EDGE('',*,*,#3656,.T.);
#4782=ORIENTED_EDGE('',*,*,#3672,.F.);
#4783=ORIENTED_EDGE('',*,*,#3691,.T.);
#4784=ORIENTED_EDGE('',*,*,#3692,.F.);
#4785=ORIENTED_EDGE('',*,*,#3691,.F.);
#4786=ORIENTED_EDGE('',*,*,#3684,.T.);
#4787=ORIENTED_EDGE('',*,*,#3666,.T.);
#4788=ORIENTED_EDGE('',*,*,#3652,.T.);
#4789=ORIENTED_EDGE('',*,*,#3662,.T.);
#4790=ORIENTED_EDGE('',*,*,#3685,.T.);
#4791=ORIENTED_EDGE('',*,*,#3690,.F.);
#4792=ORIENTED_EDGE('',*,*,#3642,.T.);
#4793=ORIENTED_EDGE('',*,*,#3645,.T.);
#4794=ORIENTED_EDGE('',*,*,#3648,.T.);
#4795=ORIENTED_EDGE('',*,*,#3651,.T.);
#4796=ORIENTED_EDGE('',*,*,#3689,.T.);
#4797=ORIENTED_EDGE('',*,*,#3688,.T.);
#4798=ORIENTED_EDGE('',*,*,#3693,.F.);
#4799=ORIENTED_EDGE('',*,*,#3694,.T.);
#4800=ORIENTED_EDGE('',*,*,#3695,.T.);
#4801=ORIENTED_EDGE('',*,*,#3694,.F.);
#4802=ORIENTED_EDGE('',*,*,#3679,.T.);
#4803=ORIENTED_EDGE('',*,*,#3682,.T.);
#4804=ORIENTED_EDGE('',*,*,#3673,.T.);
#4805=ORIENTED_EDGE('',*,*,#3676,.T.);
#4806=ORIENTED_EDGE('',*,*,#3693,.T.);
#4807=ORIENTED_EDGE('',*,*,#3692,.T.);
#4808=ORIENTED_EDGE('',*,*,#3639,.T.);
#4809=ORIENTED_EDGE('',*,*,#3636,.T.);
#4810=ORIENTED_EDGE('',*,*,#3633,.T.);
#4811=ORIENTED_EDGE('',*,*,#3630,.T.);
#4812=ORIENTED_EDGE('',*,*,#3695,.F.);
#4813=ORIENTED_EDGE('',*,*,#3686,.T.);
#4814=ORIENTED_EDGE('',*,*,#3696,.F.);
#4815=ORIENTED_EDGE('',*,*,#3697,.T.);
#4816=ORIENTED_EDGE('',*,*,#3698,.F.);
#4817=ORIENTED_EDGE('',*,*,#3697,.F.);
#4818=ORIENTED_EDGE('',*,*,#3699,.F.);
#4819=ORIENTED_EDGE('',*,*,#3700,.T.);
#4820=ORIENTED_EDGE('',*,*,#3701,.F.);
#4821=ORIENTED_EDGE('',*,*,#3700,.F.);
#4822=ORIENTED_EDGE('',*,*,#3702,.F.);
#4823=ORIENTED_EDGE('',*,*,#3703,.T.);
#4824=ORIENTED_EDGE('',*,*,#3704,.F.);
#4825=ORIENTED_EDGE('',*,*,#3703,.F.);
#4826=ORIENTED_EDGE('',*,*,#3705,.F.);
#4827=ORIENTED_EDGE('',*,*,#3706,.T.);
#4828=ORIENTED_EDGE('',*,*,#3707,.F.);
#4829=ORIENTED_EDGE('',*,*,#3706,.F.);
#4830=ORIENTED_EDGE('',*,*,#3708,.F.);
#4831=ORIENTED_EDGE('',*,*,#3709,.F.);
#4832=ORIENTED_EDGE('',*,*,#3710,.F.);
#4833=ORIENTED_EDGE('',*,*,#3711,.T.);
#4834=ORIENTED_EDGE('',*,*,#3712,.F.);
#4835=ORIENTED_EDGE('',*,*,#3711,.F.);
#4836=ORIENTED_EDGE('',*,*,#3713,.F.);
#4837=ORIENTED_EDGE('',*,*,#3714,.T.);
#4838=ORIENTED_EDGE('',*,*,#3715,.F.);
#4839=ORIENTED_EDGE('',*,*,#3714,.F.);
#4840=ORIENTED_EDGE('',*,*,#3716,.F.);
#4841=ORIENTED_EDGE('',*,*,#3717,.T.);
#4842=ORIENTED_EDGE('',*,*,#3718,.F.);
#4843=ORIENTED_EDGE('',*,*,#3717,.F.);
#4844=ORIENTED_EDGE('',*,*,#3719,.F.);
#4845=ORIENTED_EDGE('',*,*,#3709,.T.);
#4846=ORIENTED_EDGE('',*,*,#3720,.T.);
#4847=ORIENTED_EDGE('',*,*,#3721,.T.);
#4848=ORIENTED_EDGE('',*,*,#3722,.F.);
#4849=ORIENTED_EDGE('',*,*,#3723,.F.);
#4850=ORIENTED_EDGE('',*,*,#3715,.T.);
#4851=ORIENTED_EDGE('',*,*,#3718,.T.);
#4852=ORIENTED_EDGE('',*,*,#3708,.T.);
#4853=ORIENTED_EDGE('',*,*,#3712,.T.);
#4854=ORIENTED_EDGE('',*,*,#3707,.T.);
#4855=ORIENTED_EDGE('',*,*,#3704,.T.);
#4856=ORIENTED_EDGE('',*,*,#3701,.T.);
#4857=ORIENTED_EDGE('',*,*,#3698,.T.);
#4858=ORIENTED_EDGE('',*,*,#3724,.T.);
#4859=ORIENTED_EDGE('',*,*,#3723,.T.);
#4860=ORIENTED_EDGE('',*,*,#3725,.F.);
#4861=ORIENTED_EDGE('',*,*,#3726,.F.);
#4862=ORIENTED_EDGE('',*,*,#3727,.T.);
#4863=ORIENTED_EDGE('',*,*,#3726,.T.);
#4864=ORIENTED_EDGE('',*,*,#3728,.F.);
#4865=ORIENTED_EDGE('',*,*,#3729,.F.);
#4866=ORIENTED_EDGE('',*,*,#3716,.T.);
#4867=ORIENTED_EDGE('',*,*,#3713,.T.);
#4868=ORIENTED_EDGE('',*,*,#3710,.T.);
#4869=ORIENTED_EDGE('',*,*,#3719,.T.);
#4870=ORIENTED_EDGE('',*,*,#3705,.T.);
#4871=ORIENTED_EDGE('',*,*,#3702,.T.);
#4872=ORIENTED_EDGE('',*,*,#3699,.T.);
#4873=ORIENTED_EDGE('',*,*,#3696,.T.);
#4874=ORIENTED_EDGE('',*,*,#3730,.T.);
#4875=ORIENTED_EDGE('',*,*,#3729,.T.);
#4876=ORIENTED_EDGE('',*,*,#3731,.F.);
#4877=ORIENTED_EDGE('',*,*,#3721,.F.);
#4878=ORIENTED_EDGE('',*,*,#3731,.T.);
#4879=ORIENTED_EDGE('',*,*,#3728,.T.);
#4880=ORIENTED_EDGE('',*,*,#3725,.T.);
#4881=ORIENTED_EDGE('',*,*,#3722,.T.);
#4882=ORIENTED_EDGE('',*,*,#3730,.F.);
#4883=ORIENTED_EDGE('',*,*,#3720,.F.);
#4884=ORIENTED_EDGE('',*,*,#3724,.F.);
#4885=ORIENTED_EDGE('',*,*,#3727,.F.);
#4886=ORIENTED_EDGE('',*,*,#3732,.F.);
#4887=ORIENTED_EDGE('',*,*,#3733,.T.);
#4888=ORIENTED_EDGE('',*,*,#3734,.F.);
#4889=ORIENTED_EDGE('',*,*,#3733,.F.);
#4890=ORIENTED_EDGE('',*,*,#3735,.F.);
#4891=ORIENTED_EDGE('',*,*,#3736,.T.);
#4892=ORIENTED_EDGE('',*,*,#3737,.F.);
#4893=ORIENTED_EDGE('',*,*,#3736,.F.);
#4894=ORIENTED_EDGE('',*,*,#3738,.F.);
#4895=ORIENTED_EDGE('',*,*,#3739,.T.);
#4896=ORIENTED_EDGE('',*,*,#3740,.F.);
#4897=ORIENTED_EDGE('',*,*,#3739,.F.);
#4898=ORIENTED_EDGE('',*,*,#3741,.F.);
#4899=ORIENTED_EDGE('',*,*,#3742,.T.);
#4900=ORIENTED_EDGE('',*,*,#3743,.F.);
#4901=ORIENTED_EDGE('',*,*,#3742,.F.);
#4902=ORIENTED_EDGE('',*,*,#3744,.T.);
#4903=ORIENTED_EDGE('',*,*,#3745,.T.);
#4904=ORIENTED_EDGE('',*,*,#3746,.F.);
#4905=ORIENTED_EDGE('',*,*,#3747,.F.);
#4906=ORIENTED_EDGE('',*,*,#3734,.T.);
#4907=ORIENTED_EDGE('',*,*,#3737,.T.);
#4908=ORIENTED_EDGE('',*,*,#3740,.T.);
#4909=ORIENTED_EDGE('',*,*,#3743,.T.);
#4910=ORIENTED_EDGE('',*,*,#3748,.T.);
#4911=ORIENTED_EDGE('',*,*,#3747,.T.);
#4912=ORIENTED_EDGE('',*,*,#3749,.F.);
#4913=ORIENTED_EDGE('',*,*,#3750,.F.);
#4914=ORIENTED_EDGE('',*,*,#3751,.T.);
#4915=ORIENTED_EDGE('',*,*,#3750,.T.);
#4916=ORIENTED_EDGE('',*,*,#3752,.F.);
#4917=ORIENTED_EDGE('',*,*,#3753,.F.);
#4918=ORIENTED_EDGE('',*,*,#3732,.T.);
#4919=ORIENTED_EDGE('',*,*,#3735,.T.);
#4920=ORIENTED_EDGE('',*,*,#3738,.T.);
#4921=ORIENTED_EDGE('',*,*,#3741,.T.);
#4922=ORIENTED_EDGE('',*,*,#3754,.T.);
#4923=ORIENTED_EDGE('',*,*,#3753,.T.);
#4924=ORIENTED_EDGE('',*,*,#3755,.F.);
#4925=ORIENTED_EDGE('',*,*,#3745,.F.);
#4926=ORIENTED_EDGE('',*,*,#3755,.T.);
#4927=ORIENTED_EDGE('',*,*,#3752,.T.);
#4928=ORIENTED_EDGE('',*,*,#3749,.T.);
#4929=ORIENTED_EDGE('',*,*,#3746,.T.);
#4930=ORIENTED_EDGE('',*,*,#3754,.F.);
#4931=ORIENTED_EDGE('',*,*,#3744,.F.);
#4932=ORIENTED_EDGE('',*,*,#3748,.F.);
#4933=ORIENTED_EDGE('',*,*,#3751,.F.);
#4934=ORIENTED_EDGE('',*,*,#3756,.F.);
#4935=ORIENTED_EDGE('',*,*,#3757,.T.);
#4936=ORIENTED_EDGE('',*,*,#3758,.F.);
#4937=ORIENTED_EDGE('',*,*,#3757,.F.);
#4938=ORIENTED_EDGE('',*,*,#3759,.F.);
#4939=ORIENTED_EDGE('',*,*,#3760,.T.);
#4940=ORIENTED_EDGE('',*,*,#3761,.F.);
#4941=ORIENTED_EDGE('',*,*,#3760,.F.);
#4942=ORIENTED_EDGE('',*,*,#3762,.F.);
#4943=ORIENTED_EDGE('',*,*,#3763,.T.);
#4944=ORIENTED_EDGE('',*,*,#3764,.F.);
#4945=ORIENTED_EDGE('',*,*,#3763,.F.);
#4946=ORIENTED_EDGE('',*,*,#3765,.F.);
#4947=ORIENTED_EDGE('',*,*,#3766,.T.);
#4948=ORIENTED_EDGE('',*,*,#3767,.F.);
#4949=ORIENTED_EDGE('',*,*,#3766,.F.);
#4950=ORIENTED_EDGE('',*,*,#3768,.F.);
#4951=ORIENTED_EDGE('',*,*,#3769,.F.);
#4952=ORIENTED_EDGE('',*,*,#3770,.F.);
#4953=ORIENTED_EDGE('',*,*,#3771,.T.);
#4954=ORIENTED_EDGE('',*,*,#3772,.F.);
#4955=ORIENTED_EDGE('',*,*,#3771,.F.);
#4956=ORIENTED_EDGE('',*,*,#3773,.F.);
#4957=ORIENTED_EDGE('',*,*,#3774,.T.);
#4958=ORIENTED_EDGE('',*,*,#3775,.F.);
#4959=ORIENTED_EDGE('',*,*,#3774,.F.);
#4960=ORIENTED_EDGE('',*,*,#3776,.F.);
#4961=ORIENTED_EDGE('',*,*,#3777,.T.);
#4962=ORIENTED_EDGE('',*,*,#3778,.F.);
#4963=ORIENTED_EDGE('',*,*,#3777,.F.);
#4964=ORIENTED_EDGE('',*,*,#3779,.F.);
#4965=ORIENTED_EDGE('',*,*,#3769,.T.);
#4966=ORIENTED_EDGE('',*,*,#3780,.T.);
#4967=ORIENTED_EDGE('',*,*,#3781,.T.);
#4968=ORIENTED_EDGE('',*,*,#3782,.F.);
#4969=ORIENTED_EDGE('',*,*,#3783,.F.);
#4970=ORIENTED_EDGE('',*,*,#3775,.T.);
#4971=ORIENTED_EDGE('',*,*,#3778,.T.);
#4972=ORIENTED_EDGE('',*,*,#3768,.T.);
#4973=ORIENTED_EDGE('',*,*,#3772,.T.);
#4974=ORIENTED_EDGE('',*,*,#3767,.T.);
#4975=ORIENTED_EDGE('',*,*,#3764,.T.);
#4976=ORIENTED_EDGE('',*,*,#3761,.T.);
#4977=ORIENTED_EDGE('',*,*,#3758,.T.);
#4978=ORIENTED_EDGE('',*,*,#3784,.T.);
#4979=ORIENTED_EDGE('',*,*,#3783,.T.);
#4980=ORIENTED_EDGE('',*,*,#3785,.F.);
#4981=ORIENTED_EDGE('',*,*,#3786,.F.);
#4982=ORIENTED_EDGE('',*,*,#3787,.T.);
#4983=ORIENTED_EDGE('',*,*,#3786,.T.);
#4984=ORIENTED_EDGE('',*,*,#3788,.F.);
#4985=ORIENTED_EDGE('',*,*,#3789,.F.);
#4986=ORIENTED_EDGE('',*,*,#3776,.T.);
#4987=ORIENTED_EDGE('',*,*,#3773,.T.);
#4988=ORIENTED_EDGE('',*,*,#3770,.T.);
#4989=ORIENTED_EDGE('',*,*,#3779,.T.);
#4990=ORIENTED_EDGE('',*,*,#3765,.T.);
#4991=ORIENTED_EDGE('',*,*,#3762,.T.);
#4992=ORIENTED_EDGE('',*,*,#3759,.T.);
#4993=ORIENTED_EDGE('',*,*,#3756,.T.);
#4994=ORIENTED_EDGE('',*,*,#3790,.T.);
#4995=ORIENTED_EDGE('',*,*,#3789,.T.);
#4996=ORIENTED_EDGE('',*,*,#3791,.F.);
#4997=ORIENTED_EDGE('',*,*,#3781,.F.);
#4998=ORIENTED_EDGE('',*,*,#3791,.T.);
#4999=ORIENTED_EDGE('',*,*,#3788,.T.);
#5000=ORIENTED_EDGE('',*,*,#3785,.T.);
#5001=ORIENTED_EDGE('',*,*,#3782,.T.);
#5002=ORIENTED_EDGE('',*,*,#3790,.F.);
#5003=ORIENTED_EDGE('',*,*,#3780,.F.);
#5004=ORIENTED_EDGE('',*,*,#3784,.F.);
#5005=ORIENTED_EDGE('',*,*,#3787,.F.);
#5006=ORIENTED_EDGE('',*,*,#3792,.F.);
#5007=ORIENTED_EDGE('',*,*,#3793,.T.);
#5008=ORIENTED_EDGE('',*,*,#3794,.F.);
#5009=ORIENTED_EDGE('',*,*,#3795,.F.);
#5010=ORIENTED_EDGE('',*,*,#3796,.F.);
#5011=ORIENTED_EDGE('',*,*,#3797,.F.);
#5012=ORIENTED_EDGE('',*,*,#3798,.F.);
#5013=ORIENTED_EDGE('',*,*,#3799,.T.);
#5014=ORIENTED_EDGE('',*,*,#3800,.F.);
#5015=ORIENTED_EDGE('',*,*,#3799,.F.);
#5016=ORIENTED_EDGE('',*,*,#3801,.F.);
#5017=ORIENTED_EDGE('',*,*,#3793,.F.);
#5018=ORIENTED_EDGE('',*,*,#3797,.T.);
#5019=ORIENTED_EDGE('',*,*,#3802,.F.);
#5020=ORIENTED_EDGE('',*,*,#3795,.T.);
#5021=ORIENTED_EDGE('',*,*,#3803,.F.);
#5022=ORIENTED_EDGE('',*,*,#3804,.F.);
#5023=ORIENTED_EDGE('',*,*,#3805,.T.);
#5024=ORIENTED_EDGE('',*,*,#3806,.F.);
#5025=ORIENTED_EDGE('',*,*,#3805,.F.);
#5026=ORIENTED_EDGE('',*,*,#3807,.T.);
#5027=ORIENTED_EDGE('',*,*,#3803,.T.);
#5028=ORIENTED_EDGE('',*,*,#3794,.T.);
#5029=ORIENTED_EDGE('',*,*,#3801,.T.);
#5030=ORIENTED_EDGE('',*,*,#3798,.T.);
#5031=ORIENTED_EDGE('',*,*,#3802,.T.);
#5032=ORIENTED_EDGE('',*,*,#3796,.T.);
#5033=ORIENTED_EDGE('',*,*,#3800,.T.);
#5034=ORIENTED_EDGE('',*,*,#3792,.T.);
#5035=ORIENTED_EDGE('',*,*,#3804,.T.);
#5036=ORIENTED_EDGE('',*,*,#3807,.F.);
#5037=ORIENTED_EDGE('',*,*,#3808,.F.);
#5038=ORIENTED_EDGE('',*,*,#3809,.T.);
#5039=ORIENTED_EDGE('',*,*,#3806,.T.);
#5040=ORIENTED_EDGE('',*,*,#3809,.F.);
#5041=ORIENTED_EDGE('',*,*,#3808,.T.);
#5042=ORIENTED_EDGE('',*,*,#3810,.F.);
#5043=ORIENTED_EDGE('',*,*,#3811,.T.);
#5044=ORIENTED_EDGE('',*,*,#3812,.F.);
#5045=ORIENTED_EDGE('',*,*,#3813,.F.);
#5046=ORIENTED_EDGE('',*,*,#3814,.F.);
#5047=ORIENTED_EDGE('',*,*,#3815,.F.);
#5048=ORIENTED_EDGE('',*,*,#3816,.F.);
#5049=ORIENTED_EDGE('',*,*,#3817,.T.);
#5050=ORIENTED_EDGE('',*,*,#3818,.F.);
#5051=ORIENTED_EDGE('',*,*,#3817,.F.);
#5052=ORIENTED_EDGE('',*,*,#3819,.F.);
#5053=ORIENTED_EDGE('',*,*,#3811,.F.);
#5054=ORIENTED_EDGE('',*,*,#3815,.T.);
#5055=ORIENTED_EDGE('',*,*,#3820,.F.);
#5056=ORIENTED_EDGE('',*,*,#3813,.T.);
#5057=ORIENTED_EDGE('',*,*,#3821,.F.);
#5058=ORIENTED_EDGE('',*,*,#3822,.F.);
#5059=ORIENTED_EDGE('',*,*,#3823,.T.);
#5060=ORIENTED_EDGE('',*,*,#3824,.F.);
#5061=ORIENTED_EDGE('',*,*,#3823,.F.);
#5062=ORIENTED_EDGE('',*,*,#3825,.T.);
#5063=ORIENTED_EDGE('',*,*,#3821,.T.);
#5064=ORIENTED_EDGE('',*,*,#3812,.T.);
#5065=ORIENTED_EDGE('',*,*,#3819,.T.);
#5066=ORIENTED_EDGE('',*,*,#3816,.T.);
#5067=ORIENTED_EDGE('',*,*,#3820,.T.);
#5068=ORIENTED_EDGE('',*,*,#3814,.T.);
#5069=ORIENTED_EDGE('',*,*,#3818,.T.);
#5070=ORIENTED_EDGE('',*,*,#3810,.T.);
#5071=ORIENTED_EDGE('',*,*,#3822,.T.);
#5072=ORIENTED_EDGE('',*,*,#3825,.F.);
#5073=ORIENTED_EDGE('',*,*,#3826,.F.);
#5074=ORIENTED_EDGE('',*,*,#3827,.T.);
#5075=ORIENTED_EDGE('',*,*,#3824,.T.);
#5076=ORIENTED_EDGE('',*,*,#3827,.F.);
#5077=ORIENTED_EDGE('',*,*,#3826,.T.);
#5078=ORIENTED_EDGE('',*,*,#3828,.F.);
#5079=ORIENTED_EDGE('',*,*,#3829,.T.);
#5080=ORIENTED_EDGE('',*,*,#3830,.F.);
#5081=ORIENTED_EDGE('',*,*,#3831,.F.);
#5082=ORIENTED_EDGE('',*,*,#3832,.F.);
#5083=ORIENTED_EDGE('',*,*,#3833,.F.);
#5084=ORIENTED_EDGE('',*,*,#3834,.F.);
#5085=ORIENTED_EDGE('',*,*,#3835,.T.);
#5086=ORIENTED_EDGE('',*,*,#3836,.F.);
#5087=ORIENTED_EDGE('',*,*,#3835,.F.);
#5088=ORIENTED_EDGE('',*,*,#3837,.F.);
#5089=ORIENTED_EDGE('',*,*,#3829,.F.);
#5090=ORIENTED_EDGE('',*,*,#3833,.T.);
#5091=ORIENTED_EDGE('',*,*,#3838,.F.);
#5092=ORIENTED_EDGE('',*,*,#3831,.T.);
#5093=ORIENTED_EDGE('',*,*,#3839,.F.);
#5094=ORIENTED_EDGE('',*,*,#3840,.F.);
#5095=ORIENTED_EDGE('',*,*,#3841,.T.);
#5096=ORIENTED_EDGE('',*,*,#3842,.F.);
#5097=ORIENTED_EDGE('',*,*,#3841,.F.);
#5098=ORIENTED_EDGE('',*,*,#3843,.T.);
#5099=ORIENTED_EDGE('',*,*,#3839,.T.);
#5100=ORIENTED_EDGE('',*,*,#3830,.T.);
#5101=ORIENTED_EDGE('',*,*,#3837,.T.);
#5102=ORIENTED_EDGE('',*,*,#3834,.T.);
#5103=ORIENTED_EDGE('',*,*,#3838,.T.);
#5104=ORIENTED_EDGE('',*,*,#3832,.T.);
#5105=ORIENTED_EDGE('',*,*,#3836,.T.);
#5106=ORIENTED_EDGE('',*,*,#3828,.T.);
#5107=ORIENTED_EDGE('',*,*,#3840,.T.);
#5108=ORIENTED_EDGE('',*,*,#3843,.F.);
#5109=ORIENTED_EDGE('',*,*,#3844,.F.);
#5110=ORIENTED_EDGE('',*,*,#3845,.T.);
#5111=ORIENTED_EDGE('',*,*,#3842,.T.);
#5112=ORIENTED_EDGE('',*,*,#3845,.F.);
#5113=ORIENTED_EDGE('',*,*,#3844,.T.);
#5114=ORIENTED_EDGE('',*,*,#3846,.F.);
#5115=ORIENTED_EDGE('',*,*,#3847,.T.);
#5116=ORIENTED_EDGE('',*,*,#3848,.F.);
#5117=ORIENTED_EDGE('',*,*,#3849,.F.);
#5118=ORIENTED_EDGE('',*,*,#3850,.F.);
#5119=ORIENTED_EDGE('',*,*,#3851,.F.);
#5120=ORIENTED_EDGE('',*,*,#3852,.F.);
#5121=ORIENTED_EDGE('',*,*,#3853,.T.);
#5122=ORIENTED_EDGE('',*,*,#3854,.F.);
#5123=ORIENTED_EDGE('',*,*,#3853,.F.);
#5124=ORIENTED_EDGE('',*,*,#3855,.F.);
#5125=ORIENTED_EDGE('',*,*,#3847,.F.);
#5126=ORIENTED_EDGE('',*,*,#3851,.T.);
#5127=ORIENTED_EDGE('',*,*,#3856,.F.);
#5128=ORIENTED_EDGE('',*,*,#3849,.T.);
#5129=ORIENTED_EDGE('',*,*,#3857,.F.);
#5130=ORIENTED_EDGE('',*,*,#3858,.F.);
#5131=ORIENTED_EDGE('',*,*,#3859,.T.);
#5132=ORIENTED_EDGE('',*,*,#3860,.F.);
#5133=ORIENTED_EDGE('',*,*,#3859,.F.);
#5134=ORIENTED_EDGE('',*,*,#3861,.T.);
#5135=ORIENTED_EDGE('',*,*,#3857,.T.);
#5136=ORIENTED_EDGE('',*,*,#3848,.T.);
#5137=ORIENTED_EDGE('',*,*,#3855,.T.);
#5138=ORIENTED_EDGE('',*,*,#3852,.T.);
#5139=ORIENTED_EDGE('',*,*,#3856,.T.);
#5140=ORIENTED_EDGE('',*,*,#3850,.T.);
#5141=ORIENTED_EDGE('',*,*,#3854,.T.);
#5142=ORIENTED_EDGE('',*,*,#3846,.T.);
#5143=ORIENTED_EDGE('',*,*,#3858,.T.);
#5144=ORIENTED_EDGE('',*,*,#3861,.F.);
#5145=ORIENTED_EDGE('',*,*,#3862,.F.);
#5146=ORIENTED_EDGE('',*,*,#3863,.T.);
#5147=ORIENTED_EDGE('',*,*,#3860,.T.);
#5148=ORIENTED_EDGE('',*,*,#3863,.F.);
#5149=ORIENTED_EDGE('',*,*,#3862,.T.);
#5150=ORIENTED_EDGE('',*,*,#3864,.F.);
#5151=ORIENTED_EDGE('',*,*,#3865,.T.);
#5152=ORIENTED_EDGE('',*,*,#3866,.F.);
#5153=ORIENTED_EDGE('',*,*,#3865,.F.);
#5154=ORIENTED_EDGE('',*,*,#3867,.F.);
#5155=ORIENTED_EDGE('',*,*,#3868,.T.);
#5156=ORIENTED_EDGE('',*,*,#3869,.F.);
#5157=ORIENTED_EDGE('',*,*,#3868,.F.);
#5158=ORIENTED_EDGE('',*,*,#3870,.F.);
#5159=ORIENTED_EDGE('',*,*,#3871,.T.);
#5160=ORIENTED_EDGE('',*,*,#3872,.F.);
#5161=ORIENTED_EDGE('',*,*,#3871,.F.);
#5162=ORIENTED_EDGE('',*,*,#3873,.F.);
#5163=ORIENTED_EDGE('',*,*,#3874,.T.);
#5164=ORIENTED_EDGE('',*,*,#3875,.F.);
#5165=ORIENTED_EDGE('',*,*,#3874,.F.);
#5166=ORIENTED_EDGE('',*,*,#3876,.F.);
#5167=ORIENTED_EDGE('',*,*,#3877,.T.);
#5168=ORIENTED_EDGE('',*,*,#3878,.T.);
#5169=ORIENTED_EDGE('',*,*,#3877,.F.);
#5170=ORIENTED_EDGE('',*,*,#3879,.F.);
#5171=ORIENTED_EDGE('',*,*,#3880,.T.);
#5172=ORIENTED_EDGE('',*,*,#3881,.T.);
#5173=ORIENTED_EDGE('',*,*,#3880,.F.);
#5174=ORIENTED_EDGE('',*,*,#3879,.T.);
#5175=ORIENTED_EDGE('',*,*,#3876,.T.);
#5176=ORIENTED_EDGE('',*,*,#3875,.T.);
#5177=ORIENTED_EDGE('',*,*,#3872,.T.);
#5178=ORIENTED_EDGE('',*,*,#3869,.T.);
#5179=ORIENTED_EDGE('',*,*,#3866,.T.);
#5180=ORIENTED_EDGE('',*,*,#3881,.F.);
#5181=ORIENTED_EDGE('',*,*,#3878,.F.);
#5182=ORIENTED_EDGE('',*,*,#3873,.T.);
#5183=ORIENTED_EDGE('',*,*,#3870,.T.);
#5184=ORIENTED_EDGE('',*,*,#3867,.T.);
#5185=ORIENTED_EDGE('',*,*,#3864,.T.);
#5186=ORIENTED_EDGE('',*,*,#3882,.F.);
#5187=ORIENTED_EDGE('',*,*,#3883,.T.);
#5188=ORIENTED_EDGE('',*,*,#3884,.F.);
#5189=ORIENTED_EDGE('',*,*,#3883,.F.);
#5190=ORIENTED_EDGE('',*,*,#3885,.F.);
#5191=ORIENTED_EDGE('',*,*,#3886,.T.);
#5192=ORIENTED_EDGE('',*,*,#3887,.F.);
#5193=ORIENTED_EDGE('',*,*,#3886,.F.);
#5194=ORIENTED_EDGE('',*,*,#3888,.F.);
#5195=ORIENTED_EDGE('',*,*,#3889,.T.);
#5196=ORIENTED_EDGE('',*,*,#3890,.F.);
#5197=ORIENTED_EDGE('',*,*,#3889,.F.);
#5198=ORIENTED_EDGE('',*,*,#3891,.F.);
#5199=ORIENTED_EDGE('',*,*,#3892,.T.);
#5200=ORIENTED_EDGE('',*,*,#3893,.F.);
#5201=ORIENTED_EDGE('',*,*,#3892,.F.);
#5202=ORIENTED_EDGE('',*,*,#3894,.F.);
#5203=ORIENTED_EDGE('',*,*,#3895,.T.);
#5204=ORIENTED_EDGE('',*,*,#3896,.F.);
#5205=ORIENTED_EDGE('',*,*,#3895,.F.);
#5206=ORIENTED_EDGE('',*,*,#3897,.F.);
#5207=ORIENTED_EDGE('',*,*,#3898,.T.);
#5208=ORIENTED_EDGE('',*,*,#3899,.T.);
#5209=ORIENTED_EDGE('',*,*,#3898,.F.);
#5210=ORIENTED_EDGE('',*,*,#3897,.T.);
#5211=ORIENTED_EDGE('',*,*,#3884,.T.);
#5212=ORIENTED_EDGE('',*,*,#3887,.T.);
#5213=ORIENTED_EDGE('',*,*,#3890,.T.);
#5214=ORIENTED_EDGE('',*,*,#3893,.T.);
#5215=ORIENTED_EDGE('',*,*,#3896,.T.);
#5216=ORIENTED_EDGE('',*,*,#3899,.F.);
#5217=ORIENTED_EDGE('',*,*,#3882,.T.);
#5218=ORIENTED_EDGE('',*,*,#3885,.T.);
#5219=ORIENTED_EDGE('',*,*,#3888,.T.);
#5220=ORIENTED_EDGE('',*,*,#3891,.T.);
#5221=ORIENTED_EDGE('',*,*,#3894,.T.);
#5222=ORIENTED_EDGE('',*,*,#3900,.F.);
#5223=ORIENTED_EDGE('',*,*,#3901,.T.);
#5224=ORIENTED_EDGE('',*,*,#3902,.F.);
#5225=ORIENTED_EDGE('',*,*,#3901,.F.);
#5226=ORIENTED_EDGE('',*,*,#3903,.F.);
#5227=ORIENTED_EDGE('',*,*,#3904,.T.);
#5228=ORIENTED_EDGE('',*,*,#3905,.F.);
#5229=ORIENTED_EDGE('',*,*,#3906,.T.);
#5230=ORIENTED_EDGE('',*,*,#3903,.T.);
#5231=ORIENTED_EDGE('',*,*,#3906,.F.);
#5232=ORIENTED_EDGE('',*,*,#3905,.T.);
#5233=ORIENTED_EDGE('',*,*,#3902,.T.);
#5234=ORIENTED_EDGE('',*,*,#3904,.F.);
#5235=ORIENTED_EDGE('',*,*,#3907,.T.);
#5236=ORIENTED_EDGE('',*,*,#3908,.T.);
#5237=ORIENTED_EDGE('',*,*,#3907,.F.);
#5238=ORIENTED_EDGE('',*,*,#3908,.F.);
#5239=ORIENTED_EDGE('',*,*,#3900,.T.);
#5240=ORIENTED_EDGE('',*,*,#3909,.T.);
#5241=ORIENTED_EDGE('',*,*,#3910,.T.);
#5242=ORIENTED_EDGE('',*,*,#3911,.F.);
#5243=ORIENTED_EDGE('',*,*,#3912,.F.);
#5244=ORIENTED_EDGE('',*,*,#3913,.T.);
#5245=ORIENTED_EDGE('',*,*,#3912,.T.);
#5246=ORIENTED_EDGE('',*,*,#3914,.F.);
#5247=ORIENTED_EDGE('',*,*,#3915,.F.);
#5248=ORIENTED_EDGE('',*,*,#3916,.T.);
#5249=ORIENTED_EDGE('',*,*,#3915,.T.);
#5250=ORIENTED_EDGE('',*,*,#3917,.F.);
#5251=ORIENTED_EDGE('',*,*,#3918,.F.);
#5252=ORIENTED_EDGE('',*,*,#3919,.T.);
#5253=ORIENTED_EDGE('',*,*,#3918,.T.);
#5254=ORIENTED_EDGE('',*,*,#3920,.F.);
#5255=ORIENTED_EDGE('',*,*,#3910,.F.);
#5256=ORIENTED_EDGE('',*,*,#3920,.T.);
#5257=ORIENTED_EDGE('',*,*,#3917,.T.);
#5258=ORIENTED_EDGE('',*,*,#3914,.T.);
#5259=ORIENTED_EDGE('',*,*,#3911,.T.);
#5260=ORIENTED_EDGE('',*,*,#3919,.F.);
#5261=ORIENTED_EDGE('',*,*,#3909,.F.);
#5262=ORIENTED_EDGE('',*,*,#3913,.F.);
#5263=ORIENTED_EDGE('',*,*,#3916,.F.);
#5264=ORIENTED_EDGE('',*,*,#3921,.T.);
#5265=ORIENTED_EDGE('',*,*,#3922,.T.);
#5266=ORIENTED_EDGE('',*,*,#3923,.F.);
#5267=ORIENTED_EDGE('',*,*,#3924,.F.);
#5268=ORIENTED_EDGE('',*,*,#3925,.T.);
#5269=ORIENTED_EDGE('',*,*,#3924,.T.);
#5270=ORIENTED_EDGE('',*,*,#3926,.F.);
#5271=ORIENTED_EDGE('',*,*,#3927,.F.);
#5272=ORIENTED_EDGE('',*,*,#3928,.T.);
#5273=ORIENTED_EDGE('',*,*,#3927,.T.);
#5274=ORIENTED_EDGE('',*,*,#3929,.F.);
#5275=ORIENTED_EDGE('',*,*,#3930,.F.);
#5276=ORIENTED_EDGE('',*,*,#3931,.T.);
#5277=ORIENTED_EDGE('',*,*,#3930,.T.);
#5278=ORIENTED_EDGE('',*,*,#3932,.F.);
#5279=ORIENTED_EDGE('',*,*,#3922,.F.);
#5280=ORIENTED_EDGE('',*,*,#3932,.T.);
#5281=ORIENTED_EDGE('',*,*,#3929,.T.);
#5282=ORIENTED_EDGE('',*,*,#3926,.T.);
#5283=ORIENTED_EDGE('',*,*,#3923,.T.);
#5284=ORIENTED_EDGE('',*,*,#3931,.F.);
#5285=ORIENTED_EDGE('',*,*,#3921,.F.);
#5286=ORIENTED_EDGE('',*,*,#3925,.F.);
#5287=ORIENTED_EDGE('',*,*,#3928,.F.);
#5288=ORIENTED_EDGE('',*,*,#3933,.T.);
#5289=ORIENTED_EDGE('',*,*,#3934,.T.);
#5290=ORIENTED_EDGE('',*,*,#3935,.T.);
#5291=ORIENTED_EDGE('',*,*,#3936,.F.);
#5292=ORIENTED_EDGE('',*,*,#3937,.T.);
#5293=ORIENTED_EDGE('',*,*,#3938,.T.);
#5294=ORIENTED_EDGE('',*,*,#3939,.T.);
#5295=ORIENTED_EDGE('',*,*,#3934,.F.);
#5296=ORIENTED_EDGE('',*,*,#3940,.T.);
#5297=ORIENTED_EDGE('',*,*,#3941,.T.);
#5298=ORIENTED_EDGE('',*,*,#3942,.T.);
#5299=ORIENTED_EDGE('',*,*,#3938,.F.);
#5300=ORIENTED_EDGE('',*,*,#3943,.T.);
#5301=ORIENTED_EDGE('',*,*,#3944,.T.);
#5302=ORIENTED_EDGE('',*,*,#3945,.T.);
#5303=ORIENTED_EDGE('',*,*,#3941,.F.);
#5304=ORIENTED_EDGE('',*,*,#3946,.T.);
#5305=ORIENTED_EDGE('',*,*,#3947,.T.);
#5306=ORIENTED_EDGE('',*,*,#3948,.T.);
#5307=ORIENTED_EDGE('',*,*,#3944,.F.);
#5308=ORIENTED_EDGE('',*,*,#3949,.T.);
#5309=ORIENTED_EDGE('',*,*,#3936,.T.);
#5310=ORIENTED_EDGE('',*,*,#3950,.T.);
#5311=ORIENTED_EDGE('',*,*,#3947,.F.);
#5312=ORIENTED_EDGE('',*,*,#3949,.F.);
#5313=ORIENTED_EDGE('',*,*,#3946,.F.);
#5314=ORIENTED_EDGE('',*,*,#3943,.F.);
#5315=ORIENTED_EDGE('',*,*,#3940,.F.);
#5316=ORIENTED_EDGE('',*,*,#3937,.F.);
#5317=ORIENTED_EDGE('',*,*,#3933,.F.);
#5318=ORIENTED_EDGE('',*,*,#3950,.F.);
#5319=ORIENTED_EDGE('',*,*,#3935,.F.);
#5320=ORIENTED_EDGE('',*,*,#3939,.F.);
#5321=ORIENTED_EDGE('',*,*,#3942,.F.);
#5322=ORIENTED_EDGE('',*,*,#3945,.F.);
#5323=ORIENTED_EDGE('',*,*,#3948,.F.);
#5324=ORIENTED_EDGE('',*,*,#3951,.F.);
#5325=ORIENTED_EDGE('',*,*,#3952,.F.);
#5326=ORIENTED_EDGE('',*,*,#3953,.F.);
#5327=ORIENTED_EDGE('',*,*,#3954,.T.);
#5328=ORIENTED_EDGE('',*,*,#3952,.T.);
#5329=ORIENTED_EDGE('',*,*,#3954,.F.);
#5330=ORIENTED_EDGE('',*,*,#3955,.F.);
#5331=ORIENTED_EDGE('',*,*,#3956,.T.);
#5332=ORIENTED_EDGE('',*,*,#3953,.T.);
#5333=ORIENTED_EDGE('',*,*,#3956,.F.);
#5334=ORIENTED_EDGE('',*,*,#3957,.F.);
#5335=ORIENTED_EDGE('',*,*,#3958,.T.);
#5336=ORIENTED_EDGE('',*,*,#3955,.T.);
#5337=ORIENTED_EDGE('',*,*,#3958,.F.);
#5338=ORIENTED_EDGE('',*,*,#3957,.T.);
#5339=ORIENTED_EDGE('',*,*,#3959,.F.);
#5340=ORIENTED_EDGE('',*,*,#3960,.F.);
#5341=ORIENTED_EDGE('',*,*,#3961,.T.);
#5342=ORIENTED_EDGE('',*,*,#3959,.T.);
#5343=ORIENTED_EDGE('',*,*,#3961,.F.);
#5344=ORIENTED_EDGE('',*,*,#3951,.T.);
#5345=ORIENTED_EDGE('',*,*,#3962,.T.);
#5346=ORIENTED_EDGE('',*,*,#3960,.T.);
#5347=ORIENTED_EDGE('',*,*,#3962,.F.);
#5348=ORIENTED_EDGE('',*,*,#3963,.F.);
#5349=ORIENTED_EDGE('',*,*,#3964,.T.);
#5350=ORIENTED_EDGE('',*,*,#3965,.F.);
#5351=ORIENTED_EDGE('',*,*,#3964,.F.);
#5352=ORIENTED_EDGE('',*,*,#3963,.T.);
#5353=ORIENTED_EDGE('',*,*,#3966,.F.);
#5354=ORIENTED_EDGE('',*,*,#3967,.T.);
#5355=ORIENTED_EDGE('',*,*,#3968,.T.);
#5356=ORIENTED_EDGE('',*,*,#3969,.T.);
#5357=ORIENTED_EDGE('',*,*,#3970,.T.);
#5358=ORIENTED_EDGE('',*,*,#3971,.T.);
#5359=ORIENTED_EDGE('',*,*,#3972,.T.);
#5360=ORIENTED_EDGE('',*,*,#3973,.T.);
#5361=ORIENTED_EDGE('',*,*,#3974,.F.);
#5362=ORIENTED_EDGE('',*,*,#3975,.F.);
#5363=ORIENTED_EDGE('',*,*,#3976,.F.);
#5364=ORIENTED_EDGE('',*,*,#3977,.F.);
#5365=ORIENTED_EDGE('',*,*,#3978,.F.);
#5366=ORIENTED_EDGE('',*,*,#3979,.F.);
#5367=ORIENTED_EDGE('',*,*,#3980,.F.);
#5368=ORIENTED_EDGE('',*,*,#3975,.T.);
#5369=ORIENTED_EDGE('',*,*,#3981,.T.);
#5370=ORIENTED_EDGE('',*,*,#3972,.F.);
#5371=ORIENTED_EDGE('',*,*,#3982,.F.);
#5372=ORIENTED_EDGE('',*,*,#3976,.T.);
#5373=ORIENTED_EDGE('',*,*,#3982,.T.);
#5374=ORIENTED_EDGE('',*,*,#3971,.F.);
#5375=ORIENTED_EDGE('',*,*,#3983,.F.);
#5376=ORIENTED_EDGE('',*,*,#3977,.T.);
#5377=ORIENTED_EDGE('',*,*,#3983,.T.);
#5378=ORIENTED_EDGE('',*,*,#3970,.F.);
#5379=ORIENTED_EDGE('',*,*,#3984,.F.);
#5380=ORIENTED_EDGE('',*,*,#3978,.T.);
#5381=ORIENTED_EDGE('',*,*,#3984,.T.);
#5382=ORIENTED_EDGE('',*,*,#3969,.F.);
#5383=ORIENTED_EDGE('',*,*,#3985,.F.);
#5384=ORIENTED_EDGE('',*,*,#3979,.T.);
#5385=ORIENTED_EDGE('',*,*,#3985,.T.);
#5386=ORIENTED_EDGE('',*,*,#3968,.F.);
#5387=ORIENTED_EDGE('',*,*,#3986,.F.);
#5388=ORIENTED_EDGE('',*,*,#3974,.T.);
#5389=ORIENTED_EDGE('',*,*,#3986,.T.);
#5390=ORIENTED_EDGE('',*,*,#3967,.F.);
#5391=ORIENTED_EDGE('',*,*,#3981,.F.);
#5392=ORIENTED_EDGE('',*,*,#3987,.F.);
#5393=ORIENTED_EDGE('',*,*,#3965,.T.);
#5394=ORIENTED_EDGE('',*,*,#3987,.T.);
#5395=ORIENTED_EDGE('',*,*,#3988,.T.);
#5396=ORIENTED_EDGE('',*,*,#3989,.F.);
#5397=ORIENTED_EDGE('',*,*,#3988,.F.);
#5398=ORIENTED_EDGE('',*,*,#3990,.F.);
#5399=ORIENTED_EDGE('',*,*,#3989,.T.);
#5400=ORIENTED_EDGE('',*,*,#3973,.F.);
#5401=ORIENTED_EDGE('',*,*,#3991,.T.);
#5402=ORIENTED_EDGE('',*,*,#3990,.T.);
#5403=ORIENTED_EDGE('',*,*,#3991,.F.);
#5404=ORIENTED_EDGE('',*,*,#3992,.F.);
#5405=ORIENTED_EDGE('',*,*,#3993,.T.);
#5406=ORIENTED_EDGE('',*,*,#3980,.T.);
#5407=ORIENTED_EDGE('',*,*,#3993,.F.);
#5408=ORIENTED_EDGE('',*,*,#3992,.T.);
#5409=ORIENTED_EDGE('',*,*,#3994,.F.);
#5410=ORIENTED_EDGE('',*,*,#3994,.T.);
#5411=ORIENTED_EDGE('',*,*,#3995,.T.);
#5412=ORIENTED_EDGE('',*,*,#3966,.T.);
#5413=ORIENTED_EDGE('',*,*,#3995,.F.);
#5414=ORIENTED_EDGE('',*,*,#3996,.F.);
#5415=ORIENTED_EDGE('',*,*,#3997,.T.);
#5416=ORIENTED_EDGE('',*,*,#3998,.F.);
#5417=ORIENTED_EDGE('',*,*,#3999,.T.);
#5418=ORIENTED_EDGE('',*,*,#3996,.T.);
#5419=ORIENTED_EDGE('',*,*,#3999,.F.);
#5420=ORIENTED_EDGE('',*,*,#3998,.T.);
#5421=ORIENTED_EDGE('',*,*,#4000,.F.);
#5422=ORIENTED_EDGE('',*,*,#4001,.F.);
#5423=ORIENTED_EDGE('',*,*,#4002,.T.);
#5424=ORIENTED_EDGE('',*,*,#4000,.T.);
#5425=ORIENTED_EDGE('',*,*,#4002,.F.);
#5426=ORIENTED_EDGE('',*,*,#4001,.T.);
#5427=ORIENTED_EDGE('',*,*,#4003,.F.);
#5428=ORIENTED_EDGE('',*,*,#4003,.T.);
#5429=ORIENTED_EDGE('',*,*,#4004,.T.);
#5430=ORIENTED_EDGE('',*,*,#3997,.F.);
#5431=ORIENTED_EDGE('',*,*,#4004,.F.);
#5432=ORIENTED_EDGE('',*,*,#4005,.T.);
#5433=ORIENTED_EDGE('',*,*,#4006,.T.);
#5434=ORIENTED_EDGE('',*,*,#4007,.T.);
#5435=ORIENTED_EDGE('',*,*,#4008,.T.);
#5436=ORIENTED_EDGE('',*,*,#4009,.T.);
#5437=ORIENTED_EDGE('',*,*,#4010,.T.);
#5438=ORIENTED_EDGE('',*,*,#4011,.F.);
#5439=ORIENTED_EDGE('',*,*,#4012,.T.);
#5440=ORIENTED_EDGE('',*,*,#4013,.T.);
#5441=ORIENTED_EDGE('',*,*,#4014,.T.);
#5442=ORIENTED_EDGE('',*,*,#4015,.T.);
#5443=ORIENTED_EDGE('',*,*,#4016,.T.);
#5444=ORIENTED_EDGE('',*,*,#4017,.T.);
#5445=ORIENTED_EDGE('',*,*,#4018,.F.);
#5446=ORIENTED_EDGE('',*,*,#4019,.F.);
#5447=ORIENTED_EDGE('',*,*,#4017,.F.);
#5448=ORIENTED_EDGE('',*,*,#4020,.F.);
#5449=ORIENTED_EDGE('',*,*,#4006,.F.);
#5450=ORIENTED_EDGE('',*,*,#4020,.T.);
#5451=ORIENTED_EDGE('',*,*,#4016,.F.);
#5452=ORIENTED_EDGE('',*,*,#4021,.F.);
#5453=ORIENTED_EDGE('',*,*,#4007,.F.);
#5454=ORIENTED_EDGE('',*,*,#4021,.T.);
#5455=ORIENTED_EDGE('',*,*,#4015,.F.);
#5456=ORIENTED_EDGE('',*,*,#4022,.F.);
#5457=ORIENTED_EDGE('',*,*,#4008,.F.);
#5458=ORIENTED_EDGE('',*,*,#4022,.T.);
#5459=ORIENTED_EDGE('',*,*,#4014,.F.);
#5460=ORIENTED_EDGE('',*,*,#4023,.F.);
#5461=ORIENTED_EDGE('',*,*,#4009,.F.);
#5462=ORIENTED_EDGE('',*,*,#4023,.T.);
#5463=ORIENTED_EDGE('',*,*,#4013,.F.);
#5464=ORIENTED_EDGE('',*,*,#4024,.F.);
#5465=ORIENTED_EDGE('',*,*,#4010,.F.);
#5466=ORIENTED_EDGE('',*,*,#4024,.T.);
#5467=ORIENTED_EDGE('',*,*,#4012,.F.);
#5468=ORIENTED_EDGE('',*,*,#4019,.T.);
#5469=ORIENTED_EDGE('',*,*,#4005,.F.);
#5470=ORIENTED_EDGE('',*,*,#4018,.T.);
#5471=ORIENTED_EDGE('',*,*,#4025,.T.);
#5472=ORIENTED_EDGE('',*,*,#4026,.T.);
#5473=ORIENTED_EDGE('',*,*,#4025,.F.);
#5474=ORIENTED_EDGE('',*,*,#4027,.F.);
#5475=ORIENTED_EDGE('',*,*,#4028,.T.);
#5476=ORIENTED_EDGE('',*,*,#4026,.F.);
#5477=ORIENTED_EDGE('',*,*,#4029,.T.);
#5478=ORIENTED_EDGE('',*,*,#4027,.T.);
#5479=ORIENTED_EDGE('',*,*,#4029,.F.);
#5480=ORIENTED_EDGE('',*,*,#4030,.F.);
#5481=ORIENTED_EDGE('',*,*,#4031,.T.);
#5482=ORIENTED_EDGE('',*,*,#4011,.T.);
#5483=ORIENTED_EDGE('',*,*,#4031,.F.);
#5484=ORIENTED_EDGE('',*,*,#4032,.F.);
#5485=ORIENTED_EDGE('',*,*,#4033,.T.);
#5486=ORIENTED_EDGE('',*,*,#4030,.T.);
#5487=ORIENTED_EDGE('',*,*,#4033,.F.);
#5488=ORIENTED_EDGE('',*,*,#4032,.T.);
#5489=ORIENTED_EDGE('',*,*,#4034,.F.);
#5490=ORIENTED_EDGE('',*,*,#4034,.T.);
#5491=ORIENTED_EDGE('',*,*,#4035,.T.);
#5492=ORIENTED_EDGE('',*,*,#4028,.F.);
#5493=ORIENTED_EDGE('',*,*,#4035,.F.);
#5494=ORIENTED_EDGE('',*,*,#4036,.F.);
#5495=ORIENTED_EDGE('',*,*,#4037,.F.);
#5496=ORIENTED_EDGE('',*,*,#4038,.T.);
#5497=ORIENTED_EDGE('',*,*,#4036,.T.);
#5498=ORIENTED_EDGE('',*,*,#4038,.F.);
#5499=ORIENTED_EDGE('',*,*,#4039,.F.);
#5500=ORIENTED_EDGE('',*,*,#4040,.T.);
#5501=ORIENTED_EDGE('',*,*,#4037,.T.);
#5502=ORIENTED_EDGE('',*,*,#4040,.F.);
#5503=ORIENTED_EDGE('',*,*,#4041,.F.);
#5504=ORIENTED_EDGE('',*,*,#4042,.T.);
#5505=ORIENTED_EDGE('',*,*,#4039,.T.);
#5506=ORIENTED_EDGE('',*,*,#4042,.F.);
#5507=ORIENTED_EDGE('',*,*,#4041,.T.);
#5508=ORIENTED_EDGE('',*,*,#4043,.F.);
#5509=ORIENTED_EDGE('',*,*,#4044,.F.);
#5510=ORIENTED_EDGE('',*,*,#4045,.T.);
#5511=ORIENTED_EDGE('',*,*,#4043,.T.);
#5512=ORIENTED_EDGE('',*,*,#4045,.F.);
#5513=ORIENTED_EDGE('',*,*,#4046,.F.);
#5514=ORIENTED_EDGE('',*,*,#4047,.T.);
#5515=ORIENTED_EDGE('',*,*,#4044,.T.);
#5516=ORIENTED_EDGE('',*,*,#4047,.F.);
#5517=ORIENTED_EDGE('',*,*,#4048,.F.);
#5518=ORIENTED_EDGE('',*,*,#4049,.T.);
#5519=ORIENTED_EDGE('',*,*,#4046,.T.);
#5520=ORIENTED_EDGE('',*,*,#4049,.F.);
#5521=ORIENTED_EDGE('',*,*,#4048,.T.);
#5522=ORIENTED_EDGE('',*,*,#4050,.T.);
#5523=ORIENTED_EDGE('',*,*,#4051,.T.);
#5524=ORIENTED_EDGE('',*,*,#4052,.T.);
#5525=ORIENTED_EDGE('',*,*,#4053,.F.);
#5526=ORIENTED_EDGE('',*,*,#4054,.T.);
#5527=ORIENTED_EDGE('',*,*,#4055,.T.);
#5528=ORIENTED_EDGE('',*,*,#4056,.T.);
#5529=ORIENTED_EDGE('',*,*,#4051,.F.);
#5530=ORIENTED_EDGE('',*,*,#4057,.T.);
#5531=ORIENTED_EDGE('',*,*,#4058,.T.);
#5532=ORIENTED_EDGE('',*,*,#4059,.T.);
#5533=ORIENTED_EDGE('',*,*,#4055,.F.);
#5534=ORIENTED_EDGE('',*,*,#4060,.T.);
#5535=ORIENTED_EDGE('',*,*,#4061,.T.);
#5536=ORIENTED_EDGE('',*,*,#4062,.T.);
#5537=ORIENTED_EDGE('',*,*,#4058,.F.);
#5538=ORIENTED_EDGE('',*,*,#4063,.T.);
#5539=ORIENTED_EDGE('',*,*,#4064,.T.);
#5540=ORIENTED_EDGE('',*,*,#4065,.T.);
#5541=ORIENTED_EDGE('',*,*,#4061,.F.);
#5542=ORIENTED_EDGE('',*,*,#4066,.T.);
#5543=ORIENTED_EDGE('',*,*,#4053,.T.);
#5544=ORIENTED_EDGE('',*,*,#4067,.T.);
#5545=ORIENTED_EDGE('',*,*,#4064,.F.);
#5546=ORIENTED_EDGE('',*,*,#4066,.F.);
#5547=ORIENTED_EDGE('',*,*,#4063,.F.);
#5548=ORIENTED_EDGE('',*,*,#4060,.F.);
#5549=ORIENTED_EDGE('',*,*,#4057,.F.);
#5550=ORIENTED_EDGE('',*,*,#4054,.F.);
#5551=ORIENTED_EDGE('',*,*,#4050,.F.);
#5552=ORIENTED_EDGE('',*,*,#4067,.F.);
#5553=ORIENTED_EDGE('',*,*,#4052,.F.);
#5554=ORIENTED_EDGE('',*,*,#4056,.F.);
#5555=ORIENTED_EDGE('',*,*,#4059,.F.);
#5556=ORIENTED_EDGE('',*,*,#4062,.F.);
#5557=ORIENTED_EDGE('',*,*,#4065,.F.);
#5558=CYLINDRICAL_SURFACE('',#6504,0.21);
#5559=CYLINDRICAL_SURFACE('',#6507,0.21);
#5560=CYLINDRICAL_SURFACE('',#6510,0.21);
#5561=CYLINDRICAL_SURFACE('',#6513,0.21);
#5562=CYLINDRICAL_SURFACE('',#6523,0.165);
#5563=CYLINDRICAL_SURFACE('',#6527,0.5);
#5564=CYLINDRICAL_SURFACE('',#6532,0.5);
#5565=CYLINDRICAL_SURFACE('',#6537,0.275);
#5566=CYLINDRICAL_SURFACE('',#6539,0.275);
#5567=CYLINDRICAL_SURFACE('',#6548,0.165);
#5568=CYLINDRICAL_SURFACE('',#6552,0.5);
#5569=CYLINDRICAL_SURFACE('',#6557,0.5);
#5570=CYLINDRICAL_SURFACE('',#6562,0.275);
#5571=CYLINDRICAL_SURFACE('',#6564,0.275);
#5572=CYLINDRICAL_SURFACE('',#6579,0.4);
#5573=CYLINDRICAL_SURFACE('',#6584,0.4);
#5574=CYLINDRICAL_SURFACE('',#6587,0.4);
#5575=CYLINDRICAL_SURFACE('',#6597,0.4);
#5576=CYLINDRICAL_SURFACE('',#6598,0.4);
#5577=CYLINDRICAL_SURFACE('',#6600,0.4);
#5578=CYLINDRICAL_SURFACE('',#6603,0.685);
#5579=CYLINDRICAL_SURFACE('',#6607,0.15);
#5580=CYLINDRICAL_SURFACE('',#6609,0.25);
#5581=CYLINDRICAL_SURFACE('',#6613,0.2);
#5582=CYLINDRICAL_SURFACE('',#6615,0.515);
#5583=CYLINDRICAL_SURFACE('',#6619,0.15);
#5584=CYLINDRICAL_SURFACE('',#6621,0.25);
#5585=CYLINDRICAL_SURFACE('',#6625,0.2);
#5586=CYLINDRICAL_SURFACE('',#6627,0.515);
#5587=CYLINDRICAL_SURFACE('',#6631,0.15);
#5588=CYLINDRICAL_SURFACE('',#6633,0.25);
#5589=CYLINDRICAL_SURFACE('',#6637,0.2);
#5590=CYLINDRICAL_SURFACE('',#6639,0.515);
#5591=CYLINDRICAL_SURFACE('',#6643,0.15);
#5592=CYLINDRICAL_SURFACE('',#6645,0.25);
#5593=CYLINDRICAL_SURFACE('',#6649,0.2);
#5594=CYLINDRICAL_SURFACE('',#6651,0.515);
#5595=CYLINDRICAL_SURFACE('',#6655,0.3);
#5596=CYLINDRICAL_SURFACE('',#6658,0.4);
#5597=CYLINDRICAL_SURFACE('',#6663,0.4);
#5598=CYLINDRICAL_SURFACE('',#6668,0.4);
#5599=CYLINDRICAL_SURFACE('',#6673,0.4);
#5600=CYLINDRICAL_SURFACE('',#6678,0.225);
#5601=CYLINDRICAL_SURFACE('',#6680,0.225);
#5602=CYLINDRICAL_SURFACE('',#6682,0.225);
#5603=CYLINDRICAL_SURFACE('',#6684,0.225);
#5604=CYLINDRICAL_SURFACE('',#6693,0.2);
#5605=CYLINDRICAL_SURFACE('',#6696,0.3);
#5606=CYLINDRICAL_SURFACE('',#6705,0.6);
#5607=CYLINDRICAL_SURFACE('',#6711,0.3);
#5608=CYLINDRICAL_SURFACE('',#6712,0.1);
#5609=CYLINDRICAL_SURFACE('',#6716,0.3);
#5610=CYLINDRICAL_SURFACE('',#6719,0.5);
#5611=CYLINDRICAL_SURFACE('',#6725,0.2);
#5612=CYLINDRICAL_SURFACE('',#6728,0.3);
#5613=CYLINDRICAL_SURFACE('',#6737,0.6);
#5614=CYLINDRICAL_SURFACE('',#6743,0.3);
#5615=CYLINDRICAL_SURFACE('',#6744,0.1);
#5616=CYLINDRICAL_SURFACE('',#6748,0.3);
#5617=CYLINDRICAL_SURFACE('',#6751,0.5);
#5618=CYLINDRICAL_SURFACE('',#6757,0.2);
#5619=CYLINDRICAL_SURFACE('',#6760,0.3);
#5620=CYLINDRICAL_SURFACE('',#6769,0.6);
#5621=CYLINDRICAL_SURFACE('',#6775,0.3);
#5622=CYLINDRICAL_SURFACE('',#6776,0.1);
#5623=CYLINDRICAL_SURFACE('',#6780,0.3);
#5624=CYLINDRICAL_SURFACE('',#6783,0.5);
#5625=CYLINDRICAL_SURFACE('',#6789,0.2);
#5626=CYLINDRICAL_SURFACE('',#6792,0.3);
#5627=CYLINDRICAL_SURFACE('',#6801,0.6);
#5628=CYLINDRICAL_SURFACE('',#6807,0.3);
#5629=CYLINDRICAL_SURFACE('',#6808,0.1);
#5630=CYLINDRICAL_SURFACE('',#6812,0.3);
#5631=CYLINDRICAL_SURFACE('',#6815,0.5);
#5632=CYLINDRICAL_SURFACE('',#6821,0.3);
#5633=CYLINDRICAL_SURFACE('',#6827,0.3);
#5634=CYLINDRICAL_SURFACE('',#6833,0.165);
#5635=CYLINDRICAL_SURFACE('',#6837,0.165);
#5636=CYLINDRICAL_SURFACE('',#6841,0.165);
#5637=CYLINDRICAL_SURFACE('',#6845,0.165);
#5638=CYLINDRICAL_SURFACE('',#6849,0.08);
#5639=CYLINDRICAL_SURFACE('',#6851,0.08);
#5640=CYLINDRICAL_SURFACE('',#6853,0.08);
#5641=CYLINDRICAL_SURFACE('',#6855,0.08);
#5642=CYLINDRICAL_SURFACE('',#6875,0.685);
#5643=CYLINDRICAL_SURFACE('',#6878,2.5);
#5644=CYLINDRICAL_SURFACE('',#6882,3.);
#5645=CYLINDRICAL_SURFACE('',#6888,0.12);
#5646=CYLINDRICAL_SURFACE('',#6891,0.12);
#5647=CYLINDRICAL_SURFACE('',#6894,0.12);
#5648=CYLINDRICAL_SURFACE('',#6897,0.12);
#5649=CYLINDRICAL_SURFACE('',#6911,0.12);
#5650=CYLINDRICAL_SURFACE('',#6914,0.12);
#5651=CYLINDRICAL_SURFACE('',#6917,0.12);
#5652=CYLINDRICAL_SURFACE('',#6920,0.12);
#5653=CYLINDRICAL_SURFACE('',#6930,0.12);
#5654=CYLINDRICAL_SURFACE('',#6933,0.12);
#5655=CYLINDRICAL_SURFACE('',#6936,0.12);
#5656=CYLINDRICAL_SURFACE('',#6939,0.12);
#5657=CYLINDRICAL_SURFACE('',#6966,0.175);
#5658=CYLINDRICAL_SURFACE('',#6967,0.1);
#5659=CYLINDRICAL_SURFACE('',#6984,0.175);
#5660=CYLINDRICAL_SURFACE('',#6985,0.1);
#5661=CYLINDRICAL_SURFACE('',#7002,0.175);
#5662=CYLINDRICAL_SURFACE('',#7003,0.1);
#5663=CYLINDRICAL_SURFACE('',#7020,0.175);
#5664=CYLINDRICAL_SURFACE('',#7021,0.1);
#5665=CYLINDRICAL_SURFACE('',#7025,0.225);
#5666=CYLINDRICAL_SURFACE('',#7028,0.225);
#5667=CYLINDRICAL_SURFACE('',#7031,0.225);
#5668=CYLINDRICAL_SURFACE('',#7034,0.225);
#5669=CYLINDRICAL_SURFACE('',#7037,2.5);
#5670=CYLINDRICAL_SURFACE('',#7040,3.);
#5671=CYLINDRICAL_SURFACE('',#7046,0.6);
#5672=CYLINDRICAL_SURFACE('',#7049,0.225);
#5673=CYLINDRICAL_SURFACE('',#7052,0.225);
#5674=CYLINDRICAL_SURFACE('',#7055,0.225);
#5675=CYLINDRICAL_SURFACE('',#7058,0.225);
#5676=CYLINDRICAL_SURFACE('',#7061,3.);
#5677=CYLINDRICAL_SURFACE('',#7067,0.075);
#5678=CYLINDRICAL_SURFACE('',#7073,1.);
#5679=CYLINDRICAL_SURFACE('',#7076,0.6);
#5680=CYLINDRICAL_SURFACE('',#7108,0.425);
#5681=CYLINDRICAL_SURFACE('',#7116,0.24505);
#5682=CYLINDRICAL_SURFACE('',#7119,0.43);
#5683=CYLINDRICAL_SURFACE('',#7136,0.46);
#5684=CYLINDRICAL_SURFACE('',#7140,0.525);
#5685=CYLINDRICAL_SURFACE('',#7141,0.515);
#5686=CYLINDRICAL_SURFACE('',#7145,0.2);
#5687=CYLINDRICAL_SURFACE('',#7150,0.475);
#5688=CYLINDRICAL_SURFACE('',#7154,0.355);
#5689=CYLINDRICAL_SURFACE('',#7158,0.31);
#5690=CYLINDRICAL_SURFACE('',#7172,0.685);
#5691=CYLINDRICAL_SURFACE('',#7178,0.685);
#5692=CYLINDRICAL_SURFACE('',#7184,0.46);
#5693=CYLINDRICAL_SURFACE('',#7190,0.35);
#5694=CYLINDRICAL_SURFACE('',#7198,0.1954);
#5695=ADVANCED_FACE('',(#796),#5558,.F.);
#5696=ADVANCED_FACE('',(#797),#5559,.F.);
#5697=ADVANCED_FACE('',(#798),#5560,.F.);
#5698=ADVANCED_FACE('',(#799),#5561,.F.);
#5699=ADVANCED_FACE('',(#800),#570,.T.);
#5700=ADVANCED_FACE('',(#801),#571,.T.);
#5701=ADVANCED_FACE('',(#802),#572,.T.);
#5702=ADVANCED_FACE('',(#803),#573,.T.);
#5703=ADVANCED_FACE('',(#804,#402,#403,#404,#405),#574,.T.);
#5704=ADVANCED_FACE('',(#805,#406,#407,#408,#409),#575,.F.);
#5705=ADVANCED_FACE('',(#806),#5562,.F.);
#5706=ADVANCED_FACE('',(#807),#576,.T.);
#5707=ADVANCED_FACE('',(#808),#5563,.F.);
#5708=ADVANCED_FACE('',(#809,#410),#577,.T.);
#5709=ADVANCED_FACE('',(#810),#5564,.F.);
#5710=ADVANCED_FACE('',(#811,#411),#578,.T.);
#5711=ADVANCED_FACE('',(#812),#5565,.F.);
#5712=ADVANCED_FACE('',(#813),#5566,.F.);
#5713=ADVANCED_FACE('',(#814),#579,.T.);
#5714=ADVANCED_FACE('',(#815),#580,.T.);
#5715=ADVANCED_FACE('',(#816),#581,.T.);
#5716=ADVANCED_FACE('',(#817),#582,.T.);
#5717=ADVANCED_FACE('',(#818,#412,#413,#414),#583,.T.);
#5718=ADVANCED_FACE('',(#819,#415,#416),#584,.F.);
#5719=ADVANCED_FACE('',(#820),#5567,.F.);
#5720=ADVANCED_FACE('',(#821),#585,.T.);
#5721=ADVANCED_FACE('',(#822),#5568,.F.);
#5722=ADVANCED_FACE('',(#823,#417),#586,.T.);
#5723=ADVANCED_FACE('',(#824),#5569,.F.);
#5724=ADVANCED_FACE('',(#825,#418),#587,.T.);
#5725=ADVANCED_FACE('',(#826),#5570,.F.);
#5726=ADVANCED_FACE('',(#827),#5571,.F.);
#5727=ADVANCED_FACE('',(#828),#588,.T.);
#5728=ADVANCED_FACE('',(#829),#589,.T.);
#5729=ADVANCED_FACE('',(#830),#590,.T.);
#5730=ADVANCED_FACE('',(#831),#591,.T.);
#5731=ADVANCED_FACE('',(#832,#419,#420,#421),#592,.T.);
#5732=ADVANCED_FACE('',(#833,#422,#423),#593,.F.);
#5733=ADVANCED_FACE('',(#834),#594,.T.);
#5734=ADVANCED_FACE('',(#835),#595,.T.);
#5735=ADVANCED_FACE('',(#836),#596,.F.);
#5736=ADVANCED_FACE('',(#837),#5572,.F.);
#5737=ADVANCED_FACE('',(#838),#5573,.F.);
#5738=ADVANCED_FACE('',(#839),#5574,.F.);
#5739=ADVANCED_FACE('',(#840),#597,.F.);
#5740=ADVANCED_FACE('',(#841),#598,.T.);
#5741=ADVANCED_FACE('',(#842),#599,.T.);
#5742=ADVANCED_FACE('',(#843),#600,.T.);
#5743=ADVANCED_FACE('',(#844),#5575,.F.);
#5744=ADVANCED_FACE('',(#845),#5576,.F.);
#5745=ADVANCED_FACE('',(#846),#5577,.F.);
#5746=ADVANCED_FACE('',(#847),#601,.T.);
#5747=ADVANCED_FACE('',(#848),#5578,.F.);
#5748=ADVANCED_FACE('',(#849,#424),#602,.T.);
#5749=ADVANCED_FACE('',(#850),#5579,.F.);
#5750=ADVANCED_FACE('',(#851),#5580,.F.);
#5751=ADVANCED_FACE('',(#852,#425),#603,.T.);
#5752=ADVANCED_FACE('',(#853),#5581,.F.);
#5753=ADVANCED_FACE('',(#854),#5582,.F.);
#5754=ADVANCED_FACE('',(#855,#426),#604,.F.);
#5755=ADVANCED_FACE('',(#856),#5583,.F.);
#5756=ADVANCED_FACE('',(#857),#5584,.F.);
#5757=ADVANCED_FACE('',(#858,#427),#605,.T.);
#5758=ADVANCED_FACE('',(#859),#5585,.F.);
#5759=ADVANCED_FACE('',(#860),#5586,.F.);
#5760=ADVANCED_FACE('',(#861,#428),#606,.F.);
#5761=ADVANCED_FACE('',(#862),#5587,.F.);
#5762=ADVANCED_FACE('',(#863),#5588,.F.);
#5763=ADVANCED_FACE('',(#864,#429),#607,.T.);
#5764=ADVANCED_FACE('',(#865),#5589,.F.);
#5765=ADVANCED_FACE('',(#866),#5590,.F.);
#5766=ADVANCED_FACE('',(#867,#430),#608,.F.);
#5767=ADVANCED_FACE('',(#868),#5591,.F.);
#5768=ADVANCED_FACE('',(#869),#5592,.F.);
#5769=ADVANCED_FACE('',(#870,#431),#609,.T.);
#5770=ADVANCED_FACE('',(#871),#5593,.F.);
#5771=ADVANCED_FACE('',(#872),#5594,.F.);
#5772=ADVANCED_FACE('',(#873,#432),#610,.F.);
#5773=ADVANCED_FACE('',(#874,#433,#434,#435,#436),#5595,.F.);
#5774=ADVANCED_FACE('',(#875),#5596,.F.);
#5775=ADVANCED_FACE('',(#876,#437),#611,.T.);
#5776=ADVANCED_FACE('',(#877),#5597,.F.);
#5777=ADVANCED_FACE('',(#878,#438),#612,.T.);
#5778=ADVANCED_FACE('',(#879),#5598,.F.);
#5779=ADVANCED_FACE('',(#880,#439),#613,.T.);
#5780=ADVANCED_FACE('',(#881),#5599,.F.);
#5781=ADVANCED_FACE('',(#882,#440),#614,.T.);
#5782=ADVANCED_FACE('',(#883),#5600,.F.);
#5783=ADVANCED_FACE('',(#884),#5601,.F.);
#5784=ADVANCED_FACE('',(#885),#5602,.F.);
#5785=ADVANCED_FACE('',(#886),#5603,.F.);
#5786=ADVANCED_FACE('',(#887),#615,.T.);
#5787=ADVANCED_FACE('',(#888,#441),#616,.T.);
#5788=ADVANCED_FACE('',(#889,#442,#443,#444,#445),#617,.T.);
#5789=ADVANCED_FACE('',(#890,#446),#618,.T.);
#5790=ADVANCED_FACE('',(#891,#447,#448,#449,#450,#451,#452,#453,#454,#455),
#619,.T.);
#5791=ADVANCED_FACE('',(#892,#456,#457,#458,#459),#620,.F.);
#5792=ADVANCED_FACE('',(#893),#5604,.F.);
#5793=ADVANCED_FACE('',(#894),#5605,.T.);
#5794=ADVANCED_FACE('',(#895,#460),#621,.T.);
#5795=ADVANCED_FACE('',(#896,#461),#622,.F.);
#5796=ADVANCED_FACE('',(#897,#462),#623,.F.);
#5797=ADVANCED_FACE('',(#898),#5606,.T.);
#5798=ADVANCED_FACE('',(#899),#624,.T.);
#5799=ADVANCED_FACE('',(#900,#463),#625,.F.);
#5800=ADVANCED_FACE('',(#901),#5607,.T.);
#5801=ADVANCED_FACE('',(#902),#5608,.T.);
#5802=ADVANCED_FACE('',(#903),#626,.F.);
#5803=ADVANCED_FACE('',(#904),#5609,.F.);
#5804=ADVANCED_FACE('',(#905),#5610,.T.);
#5805=ADVANCED_FACE('',(#906,#464),#627,.T.);
#5806=ADVANCED_FACE('',(#907,#465),#628,.F.);
#5807=ADVANCED_FACE('',(#908),#5611,.F.);
#5808=ADVANCED_FACE('',(#909),#5612,.T.);
#5809=ADVANCED_FACE('',(#910,#466),#629,.T.);
#5810=ADVANCED_FACE('',(#911,#467),#630,.F.);
#5811=ADVANCED_FACE('',(#912,#468),#631,.F.);
#5812=ADVANCED_FACE('',(#913),#5613,.T.);
#5813=ADVANCED_FACE('',(#914),#632,.T.);
#5814=ADVANCED_FACE('',(#915,#469),#633,.F.);
#5815=ADVANCED_FACE('',(#916),#5614,.T.);
#5816=ADVANCED_FACE('',(#917),#5615,.T.);
#5817=ADVANCED_FACE('',(#918),#634,.F.);
#5818=ADVANCED_FACE('',(#919),#5616,.F.);
#5819=ADVANCED_FACE('',(#920),#5617,.T.);
#5820=ADVANCED_FACE('',(#921,#470),#635,.T.);
#5821=ADVANCED_FACE('',(#922,#471),#636,.F.);
#5822=ADVANCED_FACE('',(#923),#5618,.F.);
#5823=ADVANCED_FACE('',(#924),#5619,.T.);
#5824=ADVANCED_FACE('',(#925,#472),#637,.T.);
#5825=ADVANCED_FACE('',(#926,#473),#638,.F.);
#5826=ADVANCED_FACE('',(#927,#474),#639,.F.);
#5827=ADVANCED_FACE('',(#928),#5620,.T.);
#5828=ADVANCED_FACE('',(#929),#640,.T.);
#5829=ADVANCED_FACE('',(#930,#475),#641,.F.);
#5830=ADVANCED_FACE('',(#931),#5621,.T.);
#5831=ADVANCED_FACE('',(#932),#5622,.T.);
#5832=ADVANCED_FACE('',(#933),#642,.F.);
#5833=ADVANCED_FACE('',(#934),#5623,.F.);
#5834=ADVANCED_FACE('',(#935),#5624,.T.);
#5835=ADVANCED_FACE('',(#936,#476),#643,.T.);
#5836=ADVANCED_FACE('',(#937,#477),#644,.F.);
#5837=ADVANCED_FACE('',(#938),#5625,.F.);
#5838=ADVANCED_FACE('',(#939),#5626,.T.);
#5839=ADVANCED_FACE('',(#940,#478),#645,.T.);
#5840=ADVANCED_FACE('',(#941,#479),#646,.F.);
#5841=ADVANCED_FACE('',(#942,#480),#647,.F.);
#5842=ADVANCED_FACE('',(#943),#5627,.T.);
#5843=ADVANCED_FACE('',(#944),#648,.T.);
#5844=ADVANCED_FACE('',(#945,#481),#649,.F.);
#5845=ADVANCED_FACE('',(#946),#5628,.T.);
#5846=ADVANCED_FACE('',(#947),#5629,.T.);
#5847=ADVANCED_FACE('',(#948),#650,.F.);
#5848=ADVANCED_FACE('',(#949),#5630,.F.);
#5849=ADVANCED_FACE('',(#950),#5631,.T.);
#5850=ADVANCED_FACE('',(#951,#482),#651,.T.);
#5851=ADVANCED_FACE('',(#952,#483),#652,.F.);
#5852=ADVANCED_FACE('',(#953),#5632,.T.);
#5853=ADVANCED_FACE('',(#954),#653,.T.);
#5854=ADVANCED_FACE('',(#955),#654,.F.);
#5855=ADVANCED_FACE('',(#956),#5633,.T.);
#5856=ADVANCED_FACE('',(#957),#655,.T.);
#5857=ADVANCED_FACE('',(#958),#656,.F.);
#5858=ADVANCED_FACE('',(#959),#5634,.F.);
#5859=ADVANCED_FACE('',(#960),#657,.T.);
#5860=ADVANCED_FACE('',(#961),#5635,.F.);
#5861=ADVANCED_FACE('',(#962),#658,.T.);
#5862=ADVANCED_FACE('',(#963),#5636,.F.);
#5863=ADVANCED_FACE('',(#964),#659,.T.);
#5864=ADVANCED_FACE('',(#965),#5637,.F.);
#5865=ADVANCED_FACE('',(#966),#660,.T.);
#5866=ADVANCED_FACE('',(#967),#5638,.F.);
#5867=ADVANCED_FACE('',(#968),#5639,.F.);
#5868=ADVANCED_FACE('',(#969),#5640,.F.);
#5869=ADVANCED_FACE('',(#970),#5641,.F.);
#5870=ADVANCED_FACE('',(#971),#661,.F.);
#5871=ADVANCED_FACE('',(#972),#662,.F.);
#5872=ADVANCED_FACE('',(#973),#663,.F.);
#5873=ADVANCED_FACE('',(#974),#664,.F.);
#5874=ADVANCED_FACE('',(#975),#665,.F.);
#5875=ADVANCED_FACE('',(#976),#666,.F.);
#5876=ADVANCED_FACE('',(#977,#484,#485),#667,.F.);
#5877=ADVANCED_FACE('',(#978),#668,.F.);
#5878=ADVANCED_FACE('',(#979),#669,.F.);
#5879=ADVANCED_FACE('',(#980),#670,.F.);
#5880=ADVANCED_FACE('',(#981),#671,.F.);
#5881=ADVANCED_FACE('',(#982,#486,#487),#672,.F.);
#5882=ADVANCED_FACE('',(#983),#5642,.F.);
#5883=ADVANCED_FACE('',(#984,#488,#489,#490,#491),#5643,.F.);
#5884=ADVANCED_FACE('',(#985,#492),#673,.T.);
#5885=ADVANCED_FACE('',(#986,#493),#5644,.T.);
#5886=ADVANCED_FACE('',(#987,#494,#495,#496,#497,#498),#674,.T.);
#5887=ADVANCED_FACE('',(#988,#499),#675,.F.);
#5888=ADVANCED_FACE('',(#989),#5645,.F.);
#5889=ADVANCED_FACE('',(#990),#5646,.F.);
#5890=ADVANCED_FACE('',(#991),#5647,.F.);
#5891=ADVANCED_FACE('',(#992),#5648,.F.);
#5892=ADVANCED_FACE('',(#993),#676,.F.);
#5893=ADVANCED_FACE('',(#994),#677,.F.);
#5894=ADVANCED_FACE('',(#995),#678,.F.);
#5895=ADVANCED_FACE('',(#996),#679,.F.);
#5896=ADVANCED_FACE('',(#997,#500,#501,#502,#503,#504),#680,.T.);
#5897=ADVANCED_FACE('',(#998),#681,.T.);
#5898=ADVANCED_FACE('',(#999,#505,#506,#507,#508,#509),#682,.T.);
#5899=ADVANCED_FACE('',(#1000),#683,.T.);
#5900=ADVANCED_FACE('',(#1001),#684,.T.);
#5901=ADVANCED_FACE('',(#1002),#685,.F.);
#5902=ADVANCED_FACE('',(#1003),#5649,.F.);
#5903=ADVANCED_FACE('',(#1004),#5650,.F.);
#5904=ADVANCED_FACE('',(#1005),#5651,.F.);
#5905=ADVANCED_FACE('',(#1006),#5652,.F.);
#5906=ADVANCED_FACE('',(#1007,#510,#511,#512,#513),#686,.T.);
#5907=ADVANCED_FACE('',(#1008),#687,.T.);
#5908=ADVANCED_FACE('',(#1009,#514,#515,#516,#517),#688,.T.);
#5909=ADVANCED_FACE('',(#1010),#689,.T.);
#5910=ADVANCED_FACE('',(#1011),#690,.T.);
#5911=ADVANCED_FACE('',(#1012),#691,.F.);
#5912=ADVANCED_FACE('',(#1013),#5653,.F.);
#5913=ADVANCED_FACE('',(#1014),#5654,.F.);
#5914=ADVANCED_FACE('',(#1015),#5655,.F.);
#5915=ADVANCED_FACE('',(#1016),#5656,.F.);
#5916=ADVANCED_FACE('',(#1017),#692,.F.);
#5917=ADVANCED_FACE('',(#1018),#693,.F.);
#5918=ADVANCED_FACE('',(#1019),#694,.F.);
#5919=ADVANCED_FACE('',(#1020),#695,.F.);
#5920=ADVANCED_FACE('',(#1021,#518,#519,#520,#521,#522),#696,.T.);
#5921=ADVANCED_FACE('',(#1022),#697,.T.);
#5922=ADVANCED_FACE('',(#1023,#523,#524,#525,#526,#527),#698,.T.);
#5923=ADVANCED_FACE('',(#1024),#699,.T.);
#5924=ADVANCED_FACE('',(#1025),#700,.T.);
#5925=ADVANCED_FACE('',(#1026),#701,.F.);
#5926=ADVANCED_FACE('',(#1027),#702,.F.);
#5927=ADVANCED_FACE('',(#1028),#703,.F.);
#5928=ADVANCED_FACE('',(#1029),#704,.F.);
#5929=ADVANCED_FACE('',(#1030),#705,.F.);
#5930=ADVANCED_FACE('',(#1031),#706,.F.);
#5931=ADVANCED_FACE('',(#1032,#528),#707,.T.);
#5932=ADVANCED_FACE('',(#1033),#5657,.T.);
#5933=ADVANCED_FACE('',(#1034),#5658,.T.);
#5934=ADVANCED_FACE('',(#1035),#708,.T.);
#5935=ADVANCED_FACE('',(#1036),#709,.F.);
#5936=ADVANCED_FACE('',(#1037),#710,.F.);
#5937=ADVANCED_FACE('',(#1038),#711,.F.);
#5938=ADVANCED_FACE('',(#1039),#712,.F.);
#5939=ADVANCED_FACE('',(#1040),#713,.F.);
#5940=ADVANCED_FACE('',(#1041,#529),#714,.T.);
#5941=ADVANCED_FACE('',(#1042),#5659,.T.);
#5942=ADVANCED_FACE('',(#1043),#5660,.T.);
#5943=ADVANCED_FACE('',(#1044),#715,.T.);
#5944=ADVANCED_FACE('',(#1045),#716,.F.);
#5945=ADVANCED_FACE('',(#1046),#717,.F.);
#5946=ADVANCED_FACE('',(#1047),#718,.F.);
#5947=ADVANCED_FACE('',(#1048),#719,.F.);
#5948=ADVANCED_FACE('',(#1049),#720,.F.);
#5949=ADVANCED_FACE('',(#1050,#530),#721,.T.);
#5950=ADVANCED_FACE('',(#1051),#5661,.T.);
#5951=ADVANCED_FACE('',(#1052),#5662,.T.);
#5952=ADVANCED_FACE('',(#1053),#722,.T.);
#5953=ADVANCED_FACE('',(#1054),#723,.F.);
#5954=ADVANCED_FACE('',(#1055),#724,.F.);
#5955=ADVANCED_FACE('',(#1056),#725,.F.);
#5956=ADVANCED_FACE('',(#1057),#726,.F.);
#5957=ADVANCED_FACE('',(#1058),#727,.F.);
#5958=ADVANCED_FACE('',(#1059,#531),#728,.T.);
#5959=ADVANCED_FACE('',(#1060),#5663,.T.);
#5960=ADVANCED_FACE('',(#1061),#5664,.T.);
#5961=ADVANCED_FACE('',(#1062),#729,.T.);
#5962=ADVANCED_FACE('',(#1063),#5665,.F.);
#5963=ADVANCED_FACE('',(#1064),#5666,.F.);
#5964=ADVANCED_FACE('',(#1065),#5667,.F.);
#5965=ADVANCED_FACE('',(#1066),#5668,.F.);
#5966=ADVANCED_FACE('',(#1067),#5669,.F.);
#5967=ADVANCED_FACE('',(#1068),#5670,.T.);
#5968=ADVANCED_FACE('',(#1069,#532,#533,#534,#535,#536),#730,.T.);
#5969=ADVANCED_FACE('',(#1070,#537,#538,#539,#540,#541),#731,.F.);
#5970=ADVANCED_FACE('',(#1071),#5671,.F.);
#5971=ADVANCED_FACE('',(#1072),#5672,.F.);
#5972=ADVANCED_FACE('',(#1073),#5673,.F.);
#5973=ADVANCED_FACE('',(#1074),#5674,.F.);
#5974=ADVANCED_FACE('',(#1075),#5675,.F.);
#5975=ADVANCED_FACE('',(#1076),#5676,.T.);
#5976=ADVANCED_FACE('',(#1077,#542,#543,#544,#545,#546),#732,.T.);
#5977=ADVANCED_FACE('',(#1078,#547,#548,#549,#550,#551),#733,.F.);
#5978=ADVANCED_FACE('',(#1079),#5677,.F.);
#5979=ADVANCED_FACE('',(#1080,#552),#734,.F.);
#5980=ADVANCED_FACE('',(#1081),#5678,.T.);
#5981=ADVANCED_FACE('',(#1082,#553),#735,.T.);
#5982=ADVANCED_FACE('',(#1083),#5679,.T.);
#5983=ADVANCED_FACE('',(#1084,#554),#736,.F.);
#5984=ADVANCED_FACE('',(#1085),#737,.T.);
#5985=ADVANCED_FACE('',(#1086),#738,.T.);
#5986=ADVANCED_FACE('',(#1087),#739,.T.);
#5987=ADVANCED_FACE('',(#1088),#740,.T.);
#5988=ADVANCED_FACE('',(#1089),#741,.T.);
#5989=ADVANCED_FACE('',(#1090),#742,.F.);
#5990=ADVANCED_FACE('',(#1091),#743,.T.);
#5991=ADVANCED_FACE('',(#1092),#744,.T.);
#5992=ADVANCED_FACE('',(#1093),#745,.T.);
#5993=ADVANCED_FACE('',(#1094),#746,.T.);
#5994=ADVANCED_FACE('',(#1095),#747,.T.);
#5995=ADVANCED_FACE('',(#1096),#748,.F.);
#5996=ADVANCED_FACE('',(#1097),#749,.F.);
#5997=ADVANCED_FACE('',(#1098),#750,.F.);
#5998=ADVANCED_FACE('',(#1099),#751,.F.);
#5999=ADVANCED_FACE('',(#1100),#752,.F.);
#6000=ADVANCED_FACE('',(#1101),#753,.F.);
#6001=ADVANCED_FACE('',(#1102),#754,.F.);
#6002=ADVANCED_FACE('',(#1103),#755,.F.);
#6003=ADVANCED_FACE('',(#1104),#756,.F.);
#6004=ADVANCED_FACE('',(#1105),#757,.F.);
#6005=ADVANCED_FACE('',(#1106),#758,.T.);
#6006=ADVANCED_FACE('',(#1107),#211,.T.);
#6007=ADVANCED_FACE('',(#1108),#5680,.T.);
#6008=ADVANCED_FACE('',(#1109),#212,.T.);
#6009=ADVANCED_FACE('',(#1110,#555),#759,.T.);
#6010=ADVANCED_FACE('',(#1111),#213,.T.);
#6011=ADVANCED_FACE('',(#1112),#5681,.T.);
#6012=ADVANCED_FACE('',(#1113),#5682,.F.);
#6013=ADVANCED_FACE('',(#1114,#556),#760,.T.);
#6014=ADVANCED_FACE('',(#1115,#557),#761,.T.);
#6015=ADVANCED_FACE('',(#1116,#558),#762,.F.);
#6016=ADVANCED_FACE('',(#1117),#763,.T.);
#6017=ADVANCED_FACE('',(#1118),#764,.T.);
#6018=ADVANCED_FACE('',(#1119),#765,.T.);
#6019=ADVANCED_FACE('',(#1120),#766,.T.);
#6020=ADVANCED_FACE('',(#1121),#767,.T.);
#6021=ADVANCED_FACE('',(#1122),#768,.T.);
#6022=ADVANCED_FACE('',(#1123,#559),#769,.T.);
#6023=ADVANCED_FACE('',(#1124),#5683,.F.);
#6024=ADVANCED_FACE('',(#1125,#560),#770,.T.);
#6025=ADVANCED_FACE('',(#1126),#5684,.T.);
#6026=ADVANCED_FACE('',(#1127),#5685,.T.);
#6027=ADVANCED_FACE('',(#1128,#561),#771,.T.);
#6028=ADVANCED_FACE('',(#1129),#5686,.F.);
#6029=ADVANCED_FACE('',(#1130,#562),#772,.T.);
#6030=ADVANCED_FACE('',(#1131),#5687,.T.);
#6031=ADVANCED_FACE('',(#1132,#563),#773,.T.);
#6032=ADVANCED_FACE('',(#1133),#5688,.T.);
#6033=ADVANCED_FACE('',(#1134,#564),#774,.T.);
#6034=ADVANCED_FACE('',(#1135),#5689,.F.);
#6035=ADVANCED_FACE('',(#1136,#565),#775,.F.);
#6036=ADVANCED_FACE('',(#1137,#566),#776,.T.);
#6037=ADVANCED_FACE('',(#1138),#777,.T.);
#6038=ADVANCED_FACE('',(#1139),#778,.T.);
#6039=ADVANCED_FACE('',(#1140),#779,.T.);
#6040=ADVANCED_FACE('',(#1141),#780,.T.);
#6041=ADVANCED_FACE('',(#1142),#781,.T.);
#6042=ADVANCED_FACE('',(#1143),#782,.T.);
#6043=ADVANCED_FACE('',(#1144),#5690,.T.);
#6044=ADVANCED_FACE('',(#1145,#567),#783,.T.);
#6045=ADVANCED_FACE('',(#1146),#214,.T.);
#6046=ADVANCED_FACE('',(#1147),#5691,.T.);
#6047=ADVANCED_FACE('',(#1148),#215,.T.);
#6048=ADVANCED_FACE('',(#1149,#568),#784,.T.);
#6049=ADVANCED_FACE('',(#1150),#5692,.F.);
#6050=ADVANCED_FACE('',(#1151),#785,.T.);
#6051=ADVANCED_FACE('',(#1152),#216,.T.);
#6052=ADVANCED_FACE('',(#1153),#5693,.T.);
#6053=ADVANCED_FACE('',(#1154),#217,.T.);
#6054=ADVANCED_FACE('',(#1155,#569),#786,.T.);
#6055=ADVANCED_FACE('',(#1156),#218,.T.);
#6056=ADVANCED_FACE('',(#1157),#5694,.T.);
#6057=ADVANCED_FACE('',(#1158),#219,.T.);
#6058=ADVANCED_FACE('',(#1159),#787,.T.);
#6059=ADVANCED_FACE('',(#1160),#788,.F.);
#6060=ADVANCED_FACE('',(#1161),#789,.F.);
#6061=ADVANCED_FACE('',(#1162),#790,.F.);
#6062=ADVANCED_FACE('',(#1163),#791,.F.);
#6063=ADVANCED_FACE('',(#1164),#792,.F.);
#6064=ADVANCED_FACE('',(#1165),#793,.F.);
#6065=ADVANCED_FACE('',(#1166),#794,.F.);
#6066=ADVANCED_FACE('',(#1167),#795,.F.);
#6067=CLOSED_SHELL('',(#5695,#5696,#5697,#5698,#5699,#5700,#5701,#5702,
#5703,#5704));
#6068=CLOSED_SHELL('',(#5705,#5706,#5707,#5708,#5709,#5710,#5711,#5712,
#5713,#5714,#5715,#5716,#5717,#5718));
#6069=CLOSED_SHELL('',(#5719,#5720,#5721,#5722,#5723,#5724,#5725,#5726,
#5727,#5728,#5729,#5730,#5731,#5732));
#6070=CLOSED_SHELL('',(#5733,#5734,#5735,#5736,#5737,#5738,#5739,#5740,
#5741,#5742,#5743,#5744,#5745,#5746,#5747,#5748,#5749,#5750,#5751,#5752,
#5753,#5754,#5755,#5756,#5757,#5758,#5759,#5760,#5761,#5762,#5763,#5764,
#5765,#5766,#5767,#5768,#5769,#5770,#5771,#5772,#5773,#5774,#5775,#5776,
#5777,#5778,#5779,#5780,#5781,#5782,#5783,#5784,#5785,#5786,#5787,#5788,
#5789,#5790,#5791));
#6071=CLOSED_SHELL('',(#5792,#5793,#5794,#5795));
#6072=CLOSED_SHELL('',(#5796,#5797,#5798,#5799,#5800,#5801,#5802));
#6073=CLOSED_SHELL('',(#5803,#5804,#5805,#5806));
#6074=CLOSED_SHELL('',(#5807,#5808,#5809,#5810));
#6075=CLOSED_SHELL('',(#5811,#5812,#5813,#5814,#5815,#5816,#5817));
#6076=CLOSED_SHELL('',(#5818,#5819,#5820,#5821));
#6077=CLOSED_SHELL('',(#5822,#5823,#5824,#5825));
#6078=CLOSED_SHELL('',(#5826,#5827,#5828,#5829,#5830,#5831,#5832));
#6079=CLOSED_SHELL('',(#5833,#5834,#5835,#5836));
#6080=CLOSED_SHELL('',(#5837,#5838,#5839,#5840));
#6081=CLOSED_SHELL('',(#5841,#5842,#5843,#5844,#5845,#5846,#5847));
#6082=CLOSED_SHELL('',(#5848,#5849,#5850,#5851));
#6083=CLOSED_SHELL('',(#5852,#5853,#5854));
#6084=CLOSED_SHELL('',(#5855,#5856,#5857));
#6085=CLOSED_SHELL('',(#5858,#5859,#5860,#5861,#5862,#5863,#5864,#5865,
#5866,#5867,#5868,#5869,#5870,#5871,#5872,#5873,#5874,#5875,#5876,#5877,
#5878,#5879,#5880,#5881,#5882,#5883,#5884,#5885,#5886,#5887));
#6086=CLOSED_SHELL('',(#5888,#5889,#5890,#5891,#5892,#5893,#5894,#5895,
#5896,#5897,#5898,#5899,#5900,#5901));
#6087=CLOSED_SHELL('',(#5902,#5903,#5904,#5905,#5906,#5907,#5908,#5909,
#5910,#5911));
#6088=CLOSED_SHELL('',(#5912,#5913,#5914,#5915,#5916,#5917,#5918,#5919,
#5920,#5921,#5922,#5923,#5924,#5925));
#6089=CLOSED_SHELL('',(#5926,#5927,#5928,#5929,#5930,#5931,#5932,#5933,
#5934));
#6090=CLOSED_SHELL('',(#5935,#5936,#5937,#5938,#5939,#5940,#5941,#5942,
#5943));
#6091=CLOSED_SHELL('',(#5944,#5945,#5946,#5947,#5948,#5949,#5950,#5951,
#5952));
#6092=CLOSED_SHELL('',(#5953,#5954,#5955,#5956,#5957,#5958,#5959,#5960,
#5961));
#6093=CLOSED_SHELL('',(#5962,#5963,#5964,#5965,#5966,#5967,#5968,#5969));
#6094=CLOSED_SHELL('',(#5970,#5971,#5972,#5973,#5974,#5975,#5976,#5977));
#6095=CLOSED_SHELL('',(#5978,#5979,#5980,#5981,#5982,#5983));
#6096=CLOSED_SHELL('',(#5984,#5985,#5986,#5987,#5988,#5989));
#6097=CLOSED_SHELL('',(#5990,#5991,#5992,#5993,#5994,#5995));
#6098=CLOSED_SHELL('',(#5996,#5997,#5998,#5999,#6000,#6001,#6002,#6003));
#6099=CLOSED_SHELL('',(#6004,#6005,#6006,#6007,#6008,#6009,#6010,#6011));
#6100=CLOSED_SHELL('',(#6012,#6013,#6014,#6015,#6016,#6017,#6018,#6019,
#6020,#6021,#6022,#6023,#6024,#6025,#6026,#6027,#6028));
#6101=CLOSED_SHELL('',(#6029,#6030,#6031,#6032,#6033,#6034));
#6102=CLOSED_SHELL('',(#6035,#6036,#6037,#6038,#6039,#6040,#6041,#6042,
#6043,#6044,#6045,#6046,#6047,#6048,#6049));
#6103=CLOSED_SHELL('',(#6050,#6051,#6052,#6053,#6054,#6055,#6056,#6057,
#6058));
#6104=CLOSED_SHELL('',(#6059,#6060,#6061,#6062,#6063,#6064,#6065,#6066));
#6105=DERIVED_UNIT_ELEMENT(#6177,1.);
#6106=DERIVED_UNIT_ELEMENT(#11434,-3.);
#6107=DERIVED_UNIT_ELEMENT(#6177,1.);
#6108=DERIVED_UNIT_ELEMENT(#11434,-3.);
#6109=DERIVED_UNIT_ELEMENT(#6177,1.);
#6110=DERIVED_UNIT_ELEMENT(#11434,-3.);
#6111=DERIVED_UNIT_ELEMENT(#6177,1.);
#6112=DERIVED_UNIT_ELEMENT(#11434,-3.);
#6113=DERIVED_UNIT_ELEMENT(#6177,1.);
#6114=DERIVED_UNIT_ELEMENT(#11434,-3.);
#6115=DERIVED_UNIT_ELEMENT(#6177,1.);
#6116=DERIVED_UNIT_ELEMENT(#11434,-3.);
#6117=DERIVED_UNIT_ELEMENT(#6177,1.);
#6118=DERIVED_UNIT_ELEMENT(#11434,-3.);
#6119=DERIVED_UNIT_ELEMENT(#6177,1.);
#6120=DERIVED_UNIT_ELEMENT(#11434,-3.);
#6121=DERIVED_UNIT_ELEMENT(#6177,1.);
#6122=DERIVED_UNIT_ELEMENT(#11434,-3.);
#6123=DERIVED_UNIT_ELEMENT(#6177,1.);
#6124=DERIVED_UNIT_ELEMENT(#11434,-3.);
#6125=DERIVED_UNIT_ELEMENT(#6177,1.);
#6126=DERIVED_UNIT_ELEMENT(#11434,-3.);
#6127=DERIVED_UNIT_ELEMENT(#6177,1.);
#6128=DERIVED_UNIT_ELEMENT(#11434,-3.);
#6129=DERIVED_UNIT_ELEMENT(#6177,1.);
#6130=DERIVED_UNIT_ELEMENT(#11434,-3.);
#6131=DERIVED_UNIT_ELEMENT(#6177,1.);
#6132=DERIVED_UNIT_ELEMENT(#11434,-3.);
#6133=DERIVED_UNIT_ELEMENT(#6177,1.);
#6134=DERIVED_UNIT_ELEMENT(#11434,-3.);
#6135=DERIVED_UNIT_ELEMENT(#6177,1.);
#6136=DERIVED_UNIT_ELEMENT(#11434,-3.);
#6137=DERIVED_UNIT_ELEMENT(#6177,1.);
#6138=DERIVED_UNIT_ELEMENT(#11434,-3.);
#6139=DERIVED_UNIT_ELEMENT(#6177,1.);
#6140=DERIVED_UNIT_ELEMENT(#11434,-3.);
#6141=DERIVED_UNIT_ELEMENT(#6177,1.);
#6142=DERIVED_UNIT_ELEMENT(#11434,-3.);
#6143=DERIVED_UNIT_ELEMENT(#6177,1.);
#6144=DERIVED_UNIT_ELEMENT(#11434,-3.);
#6145=DERIVED_UNIT_ELEMENT(#6177,1.);
#6146=DERIVED_UNIT_ELEMENT(#11434,-3.);
#6147=DERIVED_UNIT_ELEMENT(#6177,1.);
#6148=DERIVED_UNIT_ELEMENT(#11434,-3.);
#6149=DERIVED_UNIT_ELEMENT(#6177,1.);
#6150=DERIVED_UNIT_ELEMENT(#11434,-3.);
#6151=DERIVED_UNIT_ELEMENT(#6177,1.);
#6152=DERIVED_UNIT_ELEMENT(#11434,-3.);
#6153=DERIVED_UNIT_ELEMENT(#6177,1.);
#6154=DERIVED_UNIT_ELEMENT(#11434,-3.);
#6155=DERIVED_UNIT_ELEMENT(#6177,1.);
#6156=DERIVED_UNIT_ELEMENT(#11434,-3.);
#6157=DERIVED_UNIT_ELEMENT(#6177,1.);
#6158=DERIVED_UNIT_ELEMENT(#11434,-3.);
#6159=DERIVED_UNIT_ELEMENT(#6177,1.);
#6160=DERIVED_UNIT_ELEMENT(#11434,-3.);
#6161=DERIVED_UNIT_ELEMENT(#6177,1.);
#6162=DERIVED_UNIT_ELEMENT(#11434,-3.);
#6163=DERIVED_UNIT_ELEMENT(#6177,1.);
#6164=DERIVED_UNIT_ELEMENT(#11434,-3.);
#6165=DERIVED_UNIT_ELEMENT(#6177,1.);
#6166=DERIVED_UNIT_ELEMENT(#11434,-3.);
#6167=DERIVED_UNIT_ELEMENT(#6177,1.);
#6168=DERIVED_UNIT_ELEMENT(#11434,-3.);
#6169=DERIVED_UNIT_ELEMENT(#6177,1.);
#6170=DERIVED_UNIT_ELEMENT(#11434,-3.);
#6171=DERIVED_UNIT_ELEMENT(#6177,1.);
#6172=DERIVED_UNIT_ELEMENT(#11434,-3.);
#6173=DERIVED_UNIT_ELEMENT(#6177,1.);
#6174=DERIVED_UNIT_ELEMENT(#11434,-3.);
#6175=DERIVED_UNIT_ELEMENT(#6177,1.);
#6176=DERIVED_UNIT_ELEMENT(#11434,-3.);
#6177=(
MASS_UNIT()
NAMED_UNIT(*)
SI_UNIT(.KILO.,.GRAM.)
);
#6178=DERIVED_UNIT((#6105,#6106));
#6179=DERIVED_UNIT((#6107,#6108));
#6180=DERIVED_UNIT((#6109,#6110));
#6181=DERIVED_UNIT((#6111,#6112));
#6182=DERIVED_UNIT((#6113,#6114));
#6183=DERIVED_UNIT((#6115,#6116));
#6184=DERIVED_UNIT((#6117,#6118));
#6185=DERIVED_UNIT((#6119,#6120));
#6186=DERIVED_UNIT((#6121,#6122));
#6187=DERIVED_UNIT((#6123,#6124));
#6188=DERIVED_UNIT((#6125,#6126));
#6189=DERIVED_UNIT((#6127,#6128));
#6190=DERIVED_UNIT((#6129,#6130));
#6191=DERIVED_UNIT((#6131,#6132));
#6192=DERIVED_UNIT((#6133,#6134));
#6193=DERIVED_UNIT((#6135,#6136));
#6194=DERIVED_UNIT((#6137,#6138));
#6195=DERIVED_UNIT((#6139,#6140));
#6196=DERIVED_UNIT((#6141,#6142));
#6197=DERIVED_UNIT((#6143,#6144));
#6198=DERIVED_UNIT((#6145,#6146));
#6199=DERIVED_UNIT((#6147,#6148));
#6200=DERIVED_UNIT((#6149,#6150));
#6201=DERIVED_UNIT((#6151,#6152));
#6202=DERIVED_UNIT((#6153,#6154));
#6203=DERIVED_UNIT((#6155,#6156));
#6204=DERIVED_UNIT((#6157,#6158));
#6205=DERIVED_UNIT((#6159,#6160));
#6206=DERIVED_UNIT((#6161,#6162));
#6207=DERIVED_UNIT((#6163,#6164));
#6208=DERIVED_UNIT((#6165,#6166));
#6209=DERIVED_UNIT((#6167,#6168));
#6210=DERIVED_UNIT((#6169,#6170));
#6211=DERIVED_UNIT((#6171,#6172));
#6212=DERIVED_UNIT((#6173,#6174));
#6213=DERIVED_UNIT((#6175,#6176));
#6214=MEASURE_REPRESENTATION_ITEM('density measure',
POSITIVE_RATIO_MEASURE(7850.),#6178);
#6215=MEASURE_REPRESENTATION_ITEM('density measure',
POSITIVE_RATIO_MEASURE(7850.),#6179);
#6216=MEASURE_REPRESENTATION_ITEM('density measure',
POSITIVE_RATIO_MEASURE(7850.),#6180);
#6217=MEASURE_REPRESENTATION_ITEM('density measure',
POSITIVE_RATIO_MEASURE(7850.),#6181);
#6218=MEASURE_REPRESENTATION_ITEM('density measure',
POSITIVE_RATIO_MEASURE(7850.),#6182);
#6219=MEASURE_REPRESENTATION_ITEM('density measure',
POSITIVE_RATIO_MEASURE(7850.),#6183);
#6220=MEASURE_REPRESENTATION_ITEM('density measure',
POSITIVE_RATIO_MEASURE(7850.),#6184);
#6221=MEASURE_REPRESENTATION_ITEM('density measure',
POSITIVE_RATIO_MEASURE(7850.),#6185);
#6222=MEASURE_REPRESENTATION_ITEM('density measure',
POSITIVE_RATIO_MEASURE(7850.),#6186);
#6223=MEASURE_REPRESENTATION_ITEM('density measure',
POSITIVE_RATIO_MEASURE(7850.),#6187);
#6224=MEASURE_REPRESENTATION_ITEM('density measure',
POSITIVE_RATIO_MEASURE(7850.),#6188);
#6225=MEASURE_REPRESENTATION_ITEM('density measure',
POSITIVE_RATIO_MEASURE(7850.),#6189);
#6226=MEASURE_REPRESENTATION_ITEM('density measure',
POSITIVE_RATIO_MEASURE(7850.),#6190);
#6227=MEASURE_REPRESENTATION_ITEM('density measure',
POSITIVE_RATIO_MEASURE(7850.),#6191);
#6228=MEASURE_REPRESENTATION_ITEM('density measure',
POSITIVE_RATIO_MEASURE(7850.),#6192);
#6229=MEASURE_REPRESENTATION_ITEM('density measure',
POSITIVE_RATIO_MEASURE(7850.),#6193);
#6230=MEASURE_REPRESENTATION_ITEM('density measure',
POSITIVE_RATIO_MEASURE(7850.),#6194);
#6231=MEASURE_REPRESENTATION_ITEM('density measure',
POSITIVE_RATIO_MEASURE(7850.),#6195);
#6232=MEASURE_REPRESENTATION_ITEM('density measure',
POSITIVE_RATIO_MEASURE(7850.),#6196);
#6233=MEASURE_REPRESENTATION_ITEM('density measure',
POSITIVE_RATIO_MEASURE(7850.),#6197);
#6234=MEASURE_REPRESENTATION_ITEM('density measure',
POSITIVE_RATIO_MEASURE(7850.),#6198);
#6235=MEASURE_REPRESENTATION_ITEM('density measure',
POSITIVE_RATIO_MEASURE(7850.),#6199);
#6236=MEASURE_REPRESENTATION_ITEM('density measure',
POSITIVE_RATIO_MEASURE(7850.),#6200);
#6237=MEASURE_REPRESENTATION_ITEM('density measure',
POSITIVE_RATIO_MEASURE(7850.),#6201);
#6238=MEASURE_REPRESENTATION_ITEM('density measure',
POSITIVE_RATIO_MEASURE(7850.),#6202);
#6239=MEASURE_REPRESENTATION_ITEM('density measure',
POSITIVE_RATIO_MEASURE(7850.),#6203);
#6240=MEASURE_REPRESENTATION_ITEM('density measure',
POSITIVE_RATIO_MEASURE(7850.),#6204);
#6241=MEASURE_REPRESENTATION_ITEM('density measure',
POSITIVE_RATIO_MEASURE(7850.),#6205);
#6242=MEASURE_REPRESENTATION_ITEM('density measure',
POSITIVE_RATIO_MEASURE(7850.),#6206);
#6243=MEASURE_REPRESENTATION_ITEM('density measure',
POSITIVE_RATIO_MEASURE(7850.),#6207);
#6244=MEASURE_REPRESENTATION_ITEM('density measure',
POSITIVE_RATIO_MEASURE(7850.),#6208);
#6245=MEASURE_REPRESENTATION_ITEM('density measure',
POSITIVE_RATIO_MEASURE(7850.),#6209);
#6246=MEASURE_REPRESENTATION_ITEM('density measure',
POSITIVE_RATIO_MEASURE(7850.),#6210);
#6247=MEASURE_REPRESENTATION_ITEM('density measure',
POSITIVE_RATIO_MEASURE(7850.),#6211);
#6248=MEASURE_REPRESENTATION_ITEM('density measure',
POSITIVE_RATIO_MEASURE(7850.),#6212);
#6249=MEASURE_REPRESENTATION_ITEM('density measure',
POSITIVE_RATIO_MEASURE(7850.),#6213);
#6250=PROPERTY_DEFINITION_REPRESENTATION(#6430,#6322);
#6251=PROPERTY_DEFINITION_REPRESENTATION(#6431,#6323);
#6252=PROPERTY_DEFINITION_REPRESENTATION(#6432,#6324);
#6253=PROPERTY_DEFINITION_REPRESENTATION(#6433,#6325);
#6254=PROPERTY_DEFINITION_REPRESENTATION(#6434,#6326);
#6255=PROPERTY_DEFINITION_REPRESENTATION(#6435,#6327);
#6256=PROPERTY_DEFINITION_REPRESENTATION(#6436,#6328);
#6257=PROPERTY_DEFINITION_REPRESENTATION(#6437,#6329);
#6258=PROPERTY_DEFINITION_REPRESENTATION(#6438,#6330);
#6259=PROPERTY_DEFINITION_REPRESENTATION(#6439,#6331);
#6260=PROPERTY_DEFINITION_REPRESENTATION(#6440,#6332);
#6261=PROPERTY_DEFINITION_REPRESENTATION(#6441,#6333);
#6262=PROPERTY_DEFINITION_REPRESENTATION(#6442,#6334);
#6263=PROPERTY_DEFINITION_REPRESENTATION(#6443,#6335);
#6264=PROPERTY_DEFINITION_REPRESENTATION(#6444,#6336);
#6265=PROPERTY_DEFINITION_REPRESENTATION(#6445,#6337);
#6266=PROPERTY_DEFINITION_REPRESENTATION(#6446,#6338);
#6267=PROPERTY_DEFINITION_REPRESENTATION(#6447,#6339);
#6268=PROPERTY_DEFINITION_REPRESENTATION(#6448,#6340);
#6269=PROPERTY_DEFINITION_REPRESENTATION(#6449,#6341);
#6270=PROPERTY_DEFINITION_REPRESENTATION(#6450,#6342);
#6271=PROPERTY_DEFINITION_REPRESENTATION(#6451,#6343);
#6272=PROPERTY_DEFINITION_REPRESENTATION(#6452,#6344);
#6273=PROPERTY_DEFINITION_REPRESENTATION(#6453,#6345);
#6274=PROPERTY_DEFINITION_REPRESENTATION(#6454,#6346);
#6275=PROPERTY_DEFINITION_REPRESENTATION(#6455,#6347);
#6276=PROPERTY_DEFINITION_REPRESENTATION(#6456,#6348);
#6277=PROPERTY_DEFINITION_REPRESENTATION(#6457,#6349);
#6278=PROPERTY_DEFINITION_REPRESENTATION(#6458,#6350);
#6279=PROPERTY_DEFINITION_REPRESENTATION(#6459,#6351);
#6280=PROPERTY_DEFINITION_REPRESENTATION(#6460,#6352);
#6281=PROPERTY_DEFINITION_REPRESENTATION(#6461,#6353);
#6282=PROPERTY_DEFINITION_REPRESENTATION(#6462,#6354);
#6283=PROPERTY_DEFINITION_REPRESENTATION(#6463,#6355);
#6284=PROPERTY_DEFINITION_REPRESENTATION(#6464,#6356);
#6285=PROPERTY_DEFINITION_REPRESENTATION(#6465,#6357);
#6286=PROPERTY_DEFINITION_REPRESENTATION(#6466,#6358);
#6287=PROPERTY_DEFINITION_REPRESENTATION(#6467,#6359);
#6288=PROPERTY_DEFINITION_REPRESENTATION(#6468,#6360);
#6289=PROPERTY_DEFINITION_REPRESENTATION(#6469,#6361);
#6290=PROPERTY_DEFINITION_REPRESENTATION(#6470,#6362);
#6291=PROPERTY_DEFINITION_REPRESENTATION(#6471,#6363);
#6292=PROPERTY_DEFINITION_REPRESENTATION(#6472,#6364);
#6293=PROPERTY_DEFINITION_REPRESENTATION(#6473,#6365);
#6294=PROPERTY_DEFINITION_REPRESENTATION(#6474,#6366);
#6295=PROPERTY_DEFINITION_REPRESENTATION(#6475,#6367);
#6296=PROPERTY_DEFINITION_REPRESENTATION(#6476,#6368);
#6297=PROPERTY_DEFINITION_REPRESENTATION(#6477,#6369);
#6298=PROPERTY_DEFINITION_REPRESENTATION(#6478,#6370);
#6299=PROPERTY_DEFINITION_REPRESENTATION(#6479,#6371);
#6300=PROPERTY_DEFINITION_REPRESENTATION(#6480,#6372);
#6301=PROPERTY_DEFINITION_REPRESENTATION(#6481,#6373);
#6302=PROPERTY_DEFINITION_REPRESENTATION(#6482,#6374);
#6303=PROPERTY_DEFINITION_REPRESENTATION(#6483,#6375);
#6304=PROPERTY_DEFINITION_REPRESENTATION(#6484,#6376);
#6305=PROPERTY_DEFINITION_REPRESENTATION(#6485,#6377);
#6306=PROPERTY_DEFINITION_REPRESENTATION(#6486,#6378);
#6307=PROPERTY_DEFINITION_REPRESENTATION(#6487,#6379);
#6308=PROPERTY_DEFINITION_REPRESENTATION(#6488,#6380);
#6309=PROPERTY_DEFINITION_REPRESENTATION(#6489,#6381);
#6310=PROPERTY_DEFINITION_REPRESENTATION(#6490,#6382);
#6311=PROPERTY_DEFINITION_REPRESENTATION(#6491,#6383);
#6312=PROPERTY_DEFINITION_REPRESENTATION(#6492,#6384);
#6313=PROPERTY_DEFINITION_REPRESENTATION(#6493,#6385);
#6314=PROPERTY_DEFINITION_REPRESENTATION(#6494,#6386);
#6315=PROPERTY_DEFINITION_REPRESENTATION(#6495,#6387);
#6316=PROPERTY_DEFINITION_REPRESENTATION(#6496,#6388);
#6317=PROPERTY_DEFINITION_REPRESENTATION(#6497,#6389);
#6318=PROPERTY_DEFINITION_REPRESENTATION(#6498,#6390);
#6319=PROPERTY_DEFINITION_REPRESENTATION(#6499,#6391);
#6320=PROPERTY_DEFINITION_REPRESENTATION(#6500,#6392);
#6321=PROPERTY_DEFINITION_REPRESENTATION(#6501,#6393);
#6322=REPRESENTATION('material name',(#6394),#11395);
#6323=REPRESENTATION('density',(#6214),#11395);
#6324=REPRESENTATION('material name',(#6395),#11396);
#6325=REPRESENTATION('density',(#6215),#11396);
#6326=REPRESENTATION('material name',(#6396),#11397);
#6327=REPRESENTATION('density',(#6216),#11397);
#6328=REPRESENTATION('material name',(#6397),#11398);
#6329=REPRESENTATION('density',(#6217),#11398);
#6330=REPRESENTATION('material name',(#6398),#11399);
#6331=REPRESENTATION('density',(#6218),#11399);
#6332=REPRESENTATION('material name',(#6399),#11400);
#6333=REPRESENTATION('density',(#6219),#11400);
#6334=REPRESENTATION('material name',(#6400),#11401);
#6335=REPRESENTATION('density',(#6220),#11401);
#6336=REPRESENTATION('material name',(#6401),#11402);
#6337=REPRESENTATION('density',(#6221),#11402);
#6338=REPRESENTATION('material name',(#6402),#11403);
#6339=REPRESENTATION('density',(#6222),#11403);
#6340=REPRESENTATION('material name',(#6403),#11404);
#6341=REPRESENTATION('density',(#6223),#11404);
#6342=REPRESENTATION('material name',(#6404),#11405);
#6343=REPRESENTATION('density',(#6224),#11405);
#6344=REPRESENTATION('material name',(#6405),#11406);
#6345=REPRESENTATION('density',(#6225),#11406);
#6346=REPRESENTATION('material name',(#6406),#11407);
#6347=REPRESENTATION('density',(#6226),#11407);
#6348=REPRESENTATION('material name',(#6407),#11408);
#6349=REPRESENTATION('density',(#6227),#11408);
#6350=REPRESENTATION('material name',(#6408),#11409);
#6351=REPRESENTATION('density',(#6228),#11409);
#6352=REPRESENTATION('material name',(#6409),#11410);
#6353=REPRESENTATION('density',(#6229),#11410);
#6354=REPRESENTATION('material name',(#6410),#11411);
#6355=REPRESENTATION('density',(#6230),#11411);
#6356=REPRESENTATION('material name',(#6411),#11412);
#6357=REPRESENTATION('density',(#6231),#11412);
#6358=REPRESENTATION('material name',(#6412),#11413);
#6359=REPRESENTATION('density',(#6232),#11413);
#6360=REPRESENTATION('material name',(#6413),#11414);
#6361=REPRESENTATION('density',(#6233),#11414);
#6362=REPRESENTATION('material name',(#6414),#11415);
#6363=REPRESENTATION('density',(#6234),#11415);
#6364=REPRESENTATION('material name',(#6415),#11416);
#6365=REPRESENTATION('density',(#6235),#11416);
#6366=REPRESENTATION('material name',(#6416),#11417);
#6367=REPRESENTATION('density',(#6236),#11417);
#6368=REPRESENTATION('material name',(#6417),#11418);
#6369=REPRESENTATION('density',(#6237),#11418);
#6370=REPRESENTATION('material name',(#6418),#11419);
#6371=REPRESENTATION('density',(#6238),#11419);
#6372=REPRESENTATION('material name',(#6419),#11420);
#6373=REPRESENTATION('density',(#6239),#11420);
#6374=REPRESENTATION('material name',(#6420),#11421);
#6375=REPRESENTATION('density',(#6240),#11421);
#6376=REPRESENTATION('material name',(#6421),#11422);
#6377=REPRESENTATION('density',(#6241),#11422);
#6378=REPRESENTATION('material name',(#6422),#11423);
#6379=REPRESENTATION('density',(#6242),#11423);
#6380=REPRESENTATION('material name',(#6423),#11424);
#6381=REPRESENTATION('density',(#6243),#11424);
#6382=REPRESENTATION('material name',(#6424),#11425);
#6383=REPRESENTATION('density',(#6244),#11425);
#6384=REPRESENTATION('material name',(#6425),#11426);
#6385=REPRESENTATION('density',(#6245),#11426);
#6386=REPRESENTATION('material name',(#6426),#11428);
#6387=REPRESENTATION('density',(#6246),#11428);
#6388=REPRESENTATION('material name',(#6427),#11429);
#6389=REPRESENTATION('density',(#6247),#11429);
#6390=REPRESENTATION('material name',(#6428),#11430);
#6391=REPRESENTATION('density',(#6248),#11430);
#6392=REPRESENTATION('material name',(#6429),#11431);
#6393=REPRESENTATION('density',(#6249),#11431);
#6394=DESCRIPTIVE_REPRESENTATION_ITEM('Steel','Steel');
#6395=DESCRIPTIVE_REPRESENTATION_ITEM('Steel','Steel');
#6396=DESCRIPTIVE_REPRESENTATION_ITEM('Steel','Steel');
#6397=DESCRIPTIVE_REPRESENTATION_ITEM('Steel','Steel');
#6398=DESCRIPTIVE_REPRESENTATION_ITEM('Steel','Steel');
#6399=DESCRIPTIVE_REPRESENTATION_ITEM('Steel','Steel');
#6400=DESCRIPTIVE_REPRESENTATION_ITEM('Steel','Steel');
#6401=DESCRIPTIVE_REPRESENTATION_ITEM('Steel','Steel');
#6402=DESCRIPTIVE_REPRESENTATION_ITEM('Steel','Steel');
#6403=DESCRIPTIVE_REPRESENTATION_ITEM('Steel','Steel');
#6404=DESCRIPTIVE_REPRESENTATION_ITEM('Steel','Steel');
#6405=DESCRIPTIVE_REPRESENTATION_ITEM('Steel','Steel');
#6406=DESCRIPTIVE_REPRESENTATION_ITEM('Steel','Steel');
#6407=DESCRIPTIVE_REPRESENTATION_ITEM('Steel','Steel');
#6408=DESCRIPTIVE_REPRESENTATION_ITEM('Steel','Steel');
#6409=DESCRIPTIVE_REPRESENTATION_ITEM('Steel','Steel');
#6410=DESCRIPTIVE_REPRESENTATION_ITEM('Steel','Steel');
#6411=DESCRIPTIVE_REPRESENTATION_ITEM('Steel','Steel');
#6412=DESCRIPTIVE_REPRESENTATION_ITEM('Steel','Steel');
#6413=DESCRIPTIVE_REPRESENTATION_ITEM('Steel','Steel');
#6414=DESCRIPTIVE_REPRESENTATION_ITEM('Steel','Steel');
#6415=DESCRIPTIVE_REPRESENTATION_ITEM('Steel','Steel');
#6416=DESCRIPTIVE_REPRESENTATION_ITEM('Steel','Steel');
#6417=DESCRIPTIVE_REPRESENTATION_ITEM('Steel','Steel');
#6418=DESCRIPTIVE_REPRESENTATION_ITEM('Steel','Steel');
#6419=DESCRIPTIVE_REPRESENTATION_ITEM('Steel','Steel');
#6420=DESCRIPTIVE_REPRESENTATION_ITEM('Steel','Steel');
#6421=DESCRIPTIVE_REPRESENTATION_ITEM('Steel','Steel');
#6422=DESCRIPTIVE_REPRESENTATION_ITEM('Steel','Steel');
#6423=DESCRIPTIVE_REPRESENTATION_ITEM('Steel','Steel');
#6424=DESCRIPTIVE_REPRESENTATION_ITEM('Steel','Steel');
#6425=DESCRIPTIVE_REPRESENTATION_ITEM('Steel','Steel');
#6426=DESCRIPTIVE_REPRESENTATION_ITEM('Steel','Steel');
#6427=DESCRIPTIVE_REPRESENTATION_ITEM('Steel','Steel');
#6428=DESCRIPTIVE_REPRESENTATION_ITEM('Steel','Steel');
#6429=DESCRIPTIVE_REPRESENTATION_ITEM('Steel','Steel');
#6430=PROPERTY_DEFINITION('material property','material name',#11603);
#6431=PROPERTY_DEFINITION('material property','density of part',#11603);
#6432=PROPERTY_DEFINITION('material property','material name',#11604);
#6433=PROPERTY_DEFINITION('material property','density of part',#11604);
#6434=PROPERTY_DEFINITION('material property','material name',#11605);
#6435=PROPERTY_DEFINITION('material property','density of part',#11605);
#6436=PROPERTY_DEFINITION('material property','material name',#11606);
#6437=PROPERTY_DEFINITION('material property','density of part',#11606);
#6438=PROPERTY_DEFINITION('material property','material name',#11607);
#6439=PROPERTY_DEFINITION('material property','density of part',#11607);
#6440=PROPERTY_DEFINITION('material property','material name',#11608);
#6441=PROPERTY_DEFINITION('material property','density of part',#11608);
#6442=PROPERTY_DEFINITION('material property','material name',#11609);
#6443=PROPERTY_DEFINITION('material property','density of part',#11609);
#6444=PROPERTY_DEFINITION('material property','material name',#11610);
#6445=PROPERTY_DEFINITION('material property','density of part',#11610);
#6446=PROPERTY_DEFINITION('material property','material name',#11611);
#6447=PROPERTY_DEFINITION('material property','density of part',#11611);
#6448=PROPERTY_DEFINITION('material property','material name',#11612);
#6449=PROPERTY_DEFINITION('material property','density of part',#11612);
#6450=PROPERTY_DEFINITION('material property','material name',#11613);
#6451=PROPERTY_DEFINITION('material property','density of part',#11613);
#6452=PROPERTY_DEFINITION('material property','material name',#11614);
#6453=PROPERTY_DEFINITION('material property','density of part',#11614);
#6454=PROPERTY_DEFINITION('material property','material name',#11615);
#6455=PROPERTY_DEFINITION('material property','density of part',#11615);
#6456=PROPERTY_DEFINITION('material property','material name',#11616);
#6457=PROPERTY_DEFINITION('material property','density of part',#11616);
#6458=PROPERTY_DEFINITION('material property','material name',#11617);
#6459=PROPERTY_DEFINITION('material property','density of part',#11617);
#6460=PROPERTY_DEFINITION('material property','material name',#11618);
#6461=PROPERTY_DEFINITION('material property','density of part',#11618);
#6462=PROPERTY_DEFINITION('material property','material name',#11619);
#6463=PROPERTY_DEFINITION('material property','density of part',#11619);
#6464=PROPERTY_DEFINITION('material property','material name',#11620);
#6465=PROPERTY_DEFINITION('material property','density of part',#11620);
#6466=PROPERTY_DEFINITION('material property','material name',#11621);
#6467=PROPERTY_DEFINITION('material property','density of part',#11621);
#6468=PROPERTY_DEFINITION('material property','material name',#11622);
#6469=PROPERTY_DEFINITION('material property','density of part',#11622);
#6470=PROPERTY_DEFINITION('material property','material name',#11623);
#6471=PROPERTY_DEFINITION('material property','density of part',#11623);
#6472=PROPERTY_DEFINITION('material property','material name',#11624);
#6473=PROPERTY_DEFINITION('material property','density of part',#11624);
#6474=PROPERTY_DEFINITION('material property','material name',#11625);
#6475=PROPERTY_DEFINITION('material property','density of part',#11625);
#6476=PROPERTY_DEFINITION('material property','material name',#11626);
#6477=PROPERTY_DEFINITION('material property','density of part',#11626);
#6478=PROPERTY_DEFINITION('material property','material name',#11627);
#6479=PROPERTY_DEFINITION('material property','density of part',#11627);
#6480=PROPERTY_DEFINITION('material property','material name',#11628);
#6481=PROPERTY_DEFINITION('material property','density of part',#11628);
#6482=PROPERTY_DEFINITION('material property','material name',#11629);
#6483=PROPERTY_DEFINITION('material property','density of part',#11629);
#6484=PROPERTY_DEFINITION('material property','material name',#11630);
#6485=PROPERTY_DEFINITION('material property','density of part',#11630);
#6486=PROPERTY_DEFINITION('material property','material name',#11631);
#6487=PROPERTY_DEFINITION('material property','density of part',#11631);
#6488=PROPERTY_DEFINITION('material property','material name',#11632);
#6489=PROPERTY_DEFINITION('material property','density of part',#11632);
#6490=PROPERTY_DEFINITION('material property','material name',#11633);
#6491=PROPERTY_DEFINITION('material property','density of part',#11633);
#6492=PROPERTY_DEFINITION('material property','material name',#11634);
#6493=PROPERTY_DEFINITION('material property','density of part',#11634);
#6494=PROPERTY_DEFINITION('material property','material name',#11636);
#6495=PROPERTY_DEFINITION('material property','density of part',#11636);
#6496=PROPERTY_DEFINITION('material property','material name',#11637);
#6497=PROPERTY_DEFINITION('material property','density of part',#11637);
#6498=PROPERTY_DEFINITION('material property','material name',#11638);
#6499=PROPERTY_DEFINITION('material property','density of part',#11638);
#6500=PROPERTY_DEFINITION('material property','material name',#11639);
#6501=PROPERTY_DEFINITION('material property','density of part',#11639);
#6502=AXIS2_PLACEMENT_3D('',#9192,#7259,#7260);
#6503=AXIS2_PLACEMENT_3D('',#9193,#7261,#7262);
#6504=AXIS2_PLACEMENT_3D('',#9194,#7263,#7264);
#6505=AXIS2_PLACEMENT_3D('',#9196,#7265,#7266);
#6506=AXIS2_PLACEMENT_3D('',#9199,#7268,#7269);
#6507=AXIS2_PLACEMENT_3D('',#9200,#7270,#7271);
#6508=AXIS2_PLACEMENT_3D('',#9202,#7272,#7273);
#6509=AXIS2_PLACEMENT_3D('',#9205,#7275,#7276);
#6510=AXIS2_PLACEMENT_3D('',#9206,#7277,#7278);
#6511=AXIS2_PLACEMENT_3D('',#9208,#7279,#7280);
#6512=AXIS2_PLACEMENT_3D('',#9211,#7282,#7283);
#6513=AXIS2_PLACEMENT_3D('',#9212,#7284,#7285);
#6514=AXIS2_PLACEMENT_3D('',#9214,#7286,#7287);
#6515=AXIS2_PLACEMENT_3D('',#9217,#7289,#7290);
#6516=AXIS2_PLACEMENT_3D('',#9218,#7291,#7292);
#6517=AXIS2_PLACEMENT_3D('',#9227,#7297,#7298);
#6518=AXIS2_PLACEMENT_3D('',#9233,#7302,#7303);
#6519=AXIS2_PLACEMENT_3D('',#9239,#7307,#7308);
#6520=AXIS2_PLACEMENT_3D('',#9242,#7311,#7312);
#6521=AXIS2_PLACEMENT_3D('',#9243,#7313,#7314);
#6522=AXIS2_PLACEMENT_3D('',#9244,#7315,#7316);
#6523=AXIS2_PLACEMENT_3D('',#9245,#7317,#7318);
#6524=AXIS2_PLACEMENT_3D('',#9247,#7319,#7320);
#6525=AXIS2_PLACEMENT_3D('',#9250,#7322,#7323);
#6526=AXIS2_PLACEMENT_3D('',#9251,#7324,#7325);
#6527=AXIS2_PLACEMENT_3D('',#9252,#7326,#7327);
#6528=AXIS2_PLACEMENT_3D('',#9254,#7328,#7329);
#6529=AXIS2_PLACEMENT_3D('',#9257,#7331,#7332);
#6530=AXIS2_PLACEMENT_3D('',#9258,#7333,#7334);
#6531=AXIS2_PLACEMENT_3D('',#9260,#7335,#7336);
#6532=AXIS2_PLACEMENT_3D('',#9261,#7337,#7338);
#6533=AXIS2_PLACEMENT_3D('',#9263,#7339,#7340);
#6534=AXIS2_PLACEMENT_3D('',#9266,#7342,#7343);
#6535=AXIS2_PLACEMENT_3D('',#9267,#7344,#7345);
#6536=AXIS2_PLACEMENT_3D('',#9269,#7346,#7347);
#6537=AXIS2_PLACEMENT_3D('',#9270,#7348,#7349);
#6538=AXIS2_PLACEMENT_3D('',#9272,#7350,#7351);
#6539=AXIS2_PLACEMENT_3D('',#9274,#7353,#7354);
#6540=AXIS2_PLACEMENT_3D('',#9276,#7355,#7356);
#6541=AXIS2_PLACEMENT_3D('',#9278,#7358,#7359);
#6542=AXIS2_PLACEMENT_3D('',#9287,#7364,#7365);
#6543=AXIS2_PLACEMENT_3D('',#9293,#7369,#7370);
#6544=AXIS2_PLACEMENT_3D('',#9299,#7374,#7375);
#6545=AXIS2_PLACEMENT_3D('',#9302,#7378,#7379);
#6546=AXIS2_PLACEMENT_3D('',#9303,#7380,#7381);
#6547=AXIS2_PLACEMENT_3D('',#9304,#7382,#7383);
#6548=AXIS2_PLACEMENT_3D('',#9305,#7384,#7385);
#6549=AXIS2_PLACEMENT_3D('',#9307,#7386,#7387);
#6550=AXIS2_PLACEMENT_3D('',#9310,#7389,#7390);
#6551=AXIS2_PLACEMENT_3D('',#9311,#7391,#7392);
#6552=AXIS2_PLACEMENT_3D('',#9312,#7393,#7394);
#6553=AXIS2_PLACEMENT_3D('',#9314,#7395,#7396);
#6554=AXIS2_PLACEMENT_3D('',#9317,#7398,#7399);
#6555=AXIS2_PLACEMENT_3D('',#9318,#7400,#7401);
#6556=AXIS2_PLACEMENT_3D('',#9320,#7402,#7403);
#6557=AXIS2_PLACEMENT_3D('',#9321,#7404,#7405);
#6558=AXIS2_PLACEMENT_3D('',#9323,#7406,#7407);
#6559=AXIS2_PLACEMENT_3D('',#9326,#7409,#7410);
#6560=AXIS2_PLACEMENT_3D('',#9327,#7411,#7412);
#6561=AXIS2_PLACEMENT_3D('',#9329,#7413,#7414);
#6562=AXIS2_PLACEMENT_3D('',#9330,#7415,#7416);
#6563=AXIS2_PLACEMENT_3D('',#9332,#7417,#7418);
#6564=AXIS2_PLACEMENT_3D('',#9334,#7420,#7421);
#6565=AXIS2_PLACEMENT_3D('',#9336,#7422,#7423);
#6566=AXIS2_PLACEMENT_3D('',#9338,#7425,#7426);
#6567=AXIS2_PLACEMENT_3D('',#9347,#7431,#7432);
#6568=AXIS2_PLACEMENT_3D('',#9353,#7436,#7437);
#6569=AXIS2_PLACEMENT_3D('',#9359,#7441,#7442);
#6570=AXIS2_PLACEMENT_3D('',#9362,#7445,#7446);
#6571=AXIS2_PLACEMENT_3D('',#9363,#7447,#7448);
#6572=AXIS2_PLACEMENT_3D('',#9364,#7449,#7450);
#6573=AXIS2_PLACEMENT_3D('',#9365,#7451,#7452);
#6574=AXIS2_PLACEMENT_3D('',#9369,#7454,#7455);
#6575=AXIS2_PLACEMENT_3D('',#9370,#7456,#7457);
#6576=AXIS2_PLACEMENT_3D('',#9373,#7459,#7460);
#6577=AXIS2_PLACEMENT_3D('',#9374,#7461,#7462);
#6578=AXIS2_PLACEMENT_3D('',#9378,#7464,#7465);
#6579=AXIS2_PLACEMENT_3D('',#9379,#7466,#7467);
#6580=AXIS2_PLACEMENT_3D('',#9385,#7470,#7471);
#6581=AXIS2_PLACEMENT_3D('',#9387,#7472,#7473);
#6582=AXIS2_PLACEMENT_3D('',#9445,#7475,#7476);
#6583=AXIS2_PLACEMENT_3D('',#9463,#7477,#7478);
#6584=AXIS2_PLACEMENT_3D('',#9464,#7479,#7480);
#6585=AXIS2_PLACEMENT_3D('',#9465,#7481,#7482);
#6586=AXIS2_PLACEMENT_3D('',#9466,#7483,#7484);
#6587=AXIS2_PLACEMENT_3D('',#9467,#7485,#7486);
#6588=AXIS2_PLACEMENT_3D('',#9469,#7487,#7488);
#6589=AXIS2_PLACEMENT_3D('',#9470,#7489,#7490);
#6590=AXIS2_PLACEMENT_3D('',#9471,#7491,#7492);
#6591=AXIS2_PLACEMENT_3D('',#9472,#7493,#7494);
#6592=AXIS2_PLACEMENT_3D('',#9474,#7496,#7497);
#6593=AXIS2_PLACEMENT_3D('',#9476,#7499,#7500);
#6594=AXIS2_PLACEMENT_3D('',#9477,#7501,#7502);
#6595=AXIS2_PLACEMENT_3D('',#9478,#7503,#7504);
#6596=AXIS2_PLACEMENT_3D('',#9479,#7505,#7506);
#6597=AXIS2_PLACEMENT_3D('',#9480,#7507,#7508);
#6598=AXIS2_PLACEMENT_3D('',#9481,#7509,#7510);
#6599=AXIS2_PLACEMENT_3D('',#9484,#7512,#7513);
#6600=AXIS2_PLACEMENT_3D('',#9485,#7514,#7515);
#6601=AXIS2_PLACEMENT_3D('',#9486,#7516,#7517);
#6602=AXIS2_PLACEMENT_3D('',#9487,#7518,#7519);
#6603=AXIS2_PLACEMENT_3D('',#9488,#7520,#7521);
#6604=AXIS2_PLACEMENT_3D('',#9490,#7522,#7523);
#6605=AXIS2_PLACEMENT_3D('',#9493,#7525,#7526);
#6606=AXIS2_PLACEMENT_3D('',#9494,#7527,#7528);
#6607=AXIS2_PLACEMENT_3D('',#9495,#7529,#7530);
#6608=AXIS2_PLACEMENT_3D('',#9521,#7532,#7533);
#6609=AXIS2_PLACEMENT_3D('',#9540,#7534,#7535);
#6610=AXIS2_PLACEMENT_3D('',#9542,#7536,#7537);
#6611=AXIS2_PLACEMENT_3D('',#9545,#7539,#7540);
#6612=AXIS2_PLACEMENT_3D('',#9546,#7541,#7542);
#6613=AXIS2_PLACEMENT_3D('',#9547,#7543,#7544);
#6614=AXIS2_PLACEMENT_3D('',#9549,#7545,#7546);
#6615=AXIS2_PLACEMENT_3D('',#9589,#7548,#7549);
#6616=AXIS2_PLACEMENT_3D('',#9591,#7550,#7551);
#6617=AXIS2_PLACEMENT_3D('',#9594,#7553,#7554);
#6618=AXIS2_PLACEMENT_3D('',#9595,#7555,#7556);
#6619=AXIS2_PLACEMENT_3D('',#9596,#7557,#7558);
#6620=AXIS2_PLACEMENT_3D('',#9622,#7560,#7561);
#6621=AXIS2_PLACEMENT_3D('',#9641,#7562,#7563);
#6622=AXIS2_PLACEMENT_3D('',#9643,#7564,#7565);
#6623=AXIS2_PLACEMENT_3D('',#9646,#7567,#7568);
#6624=AXIS2_PLACEMENT_3D('',#9647,#7569,#7570);
#6625=AXIS2_PLACEMENT_3D('',#9648,#7571,#7572);
#6626=AXIS2_PLACEMENT_3D('',#9650,#7573,#7574);
#6627=AXIS2_PLACEMENT_3D('',#9690,#7576,#7577);
#6628=AXIS2_PLACEMENT_3D('',#9692,#7578,#7579);
#6629=AXIS2_PLACEMENT_3D('',#9695,#7581,#7582);
#6630=AXIS2_PLACEMENT_3D('',#9696,#7583,#7584);
#6631=AXIS2_PLACEMENT_3D('',#9697,#7585,#7586);
#6632=AXIS2_PLACEMENT_3D('',#9723,#7588,#7589);
#6633=AXIS2_PLACEMENT_3D('',#9742,#7590,#7591);
#6634=AXIS2_PLACEMENT_3D('',#9744,#7592,#7593);
#6635=AXIS2_PLACEMENT_3D('',#9747,#7595,#7596);
#6636=AXIS2_PLACEMENT_3D('',#9748,#7597,#7598);
#6637=AXIS2_PLACEMENT_3D('',#9749,#7599,#7600);
#6638=AXIS2_PLACEMENT_3D('',#9751,#7601,#7602);
#6639=AXIS2_PLACEMENT_3D('',#9791,#7604,#7605);
#6640=AXIS2_PLACEMENT_3D('',#9793,#7606,#7607);
#6641=AXIS2_PLACEMENT_3D('',#9796,#7609,#7610);
#6642=AXIS2_PLACEMENT_3D('',#9797,#7611,#7612);
#6643=AXIS2_PLACEMENT_3D('',#9798,#7613,#7614);
#6644=AXIS2_PLACEMENT_3D('',#9824,#7616,#7617);
#6645=AXIS2_PLACEMENT_3D('',#9843,#7618,#7619);
#6646=AXIS2_PLACEMENT_3D('',#9845,#7620,#7621);
#6647=AXIS2_PLACEMENT_3D('',#9848,#7623,#7624);
#6648=AXIS2_PLACEMENT_3D('',#9849,#7625,#7626);
#6649=AXIS2_PLACEMENT_3D('',#9850,#7627,#7628);
#6650=AXIS2_PLACEMENT_3D('',#9852,#7629,#7630);
#6651=AXIS2_PLACEMENT_3D('',#9892,#7632,#7633);
#6652=AXIS2_PLACEMENT_3D('',#9894,#7634,#7635);
#6653=AXIS2_PLACEMENT_3D('',#9897,#7637,#7638);
#6654=AXIS2_PLACEMENT_3D('',#9898,#7639,#7640);
#6655=AXIS2_PLACEMENT_3D('',#9899,#7641,#7642);
#6656=AXIS2_PLACEMENT_3D('',#9901,#7643,#7644);
#6657=AXIS2_PLACEMENT_3D('',#9909,#7651,#7652);
#6658=AXIS2_PLACEMENT_3D('',#9910,#7653,#7654);
#6659=AXIS2_PLACEMENT_3D('',#9912,#7655,#7656);
#6660=AXIS2_PLACEMENT_3D('',#9915,#7658,#7659);
#6661=AXIS2_PLACEMENT_3D('',#9916,#7660,#7661);
#6662=AXIS2_PLACEMENT_3D('',#9918,#7662,#7663);
#6663=AXIS2_PLACEMENT_3D('',#9919,#7664,#7665);
#6664=AXIS2_PLACEMENT_3D('',#9921,#7666,#7667);
#6665=AXIS2_PLACEMENT_3D('',#9924,#7669,#7670);
#6666=AXIS2_PLACEMENT_3D('',#9925,#7671,#7672);
#6667=AXIS2_PLACEMENT_3D('',#9927,#7673,#7674);
#6668=AXIS2_PLACEMENT_3D('',#9928,#7675,#7676);
#6669=AXIS2_PLACEMENT_3D('',#9930,#7677,#7678);
#6670=AXIS2_PLACEMENT_3D('',#9933,#7680,#7681);
#6671=AXIS2_PLACEMENT_3D('',#9934,#7682,#7683);
#6672=AXIS2_PLACEMENT_3D('',#9936,#7684,#7685);
#6673=AXIS2_PLACEMENT_3D('',#9937,#7686,#7687);
#6674=AXIS2_PLACEMENT_3D('',#9939,#7688,#7689);
#6675=AXIS2_PLACEMENT_3D('',#9942,#7691,#7692);
#6676=AXIS2_PLACEMENT_3D('',#9943,#7693,#7694);
#6677=AXIS2_PLACEMENT_3D('',#9945,#7695,#7696);
#6678=AXIS2_PLACEMENT_3D('',#9946,#7697,#7698);
#6679=AXIS2_PLACEMENT_3D('',#9948,#7699,#7700);
#6680=AXIS2_PLACEMENT_3D('',#9950,#7702,#7703);
#6681=AXIS2_PLACEMENT_3D('',#9952,#7704,#7705);
#6682=AXIS2_PLACEMENT_3D('',#9954,#7707,#7708);
#6683=AXIS2_PLACEMENT_3D('',#9956,#7709,#7710);
#6684=AXIS2_PLACEMENT_3D('',#9958,#7712,#7713);
#6685=AXIS2_PLACEMENT_3D('',#9960,#7714,#7715);
#6686=AXIS2_PLACEMENT_3D('',#9962,#7717,#7718);
#6687=AXIS2_PLACEMENT_3D('',#9971,#7723,#7724);
#6688=AXIS2_PLACEMENT_3D('',#9977,#7728,#7729);
#6689=AXIS2_PLACEMENT_3D('',#9983,#7733,#7734);
#6690=AXIS2_PLACEMENT_3D('',#9986,#7737,#7738);
#6691=AXIS2_PLACEMENT_3D('',#9987,#7739,#7740);
#6692=AXIS2_PLACEMENT_3D('',#9988,#7741,#7742);
#6693=AXIS2_PLACEMENT_3D('',#9989,#7743,#7744);
#6694=AXIS2_PLACEMENT_3D('',#9991,#7745,#7746);
#6695=AXIS2_PLACEMENT_3D('',#9994,#7748,#7749);
#6696=AXIS2_PLACEMENT_3D('',#9995,#7750,#7751);
#6697=AXIS2_PLACEMENT_3D('',#9997,#7752,#7753);
#6698=AXIS2_PLACEMENT_3D('',#10000,#7755,#7756);
#6699=AXIS2_PLACEMENT_3D('',#10001,#7757,#7758);
#6700=AXIS2_PLACEMENT_3D('',#10002,#7759,#7760);
#6701=AXIS2_PLACEMENT_3D('',#10003,#7761,#7762);
#6702=AXIS2_PLACEMENT_3D('',#10004,#7763,#7764);
#6703=AXIS2_PLACEMENT_3D('',#10006,#7765,#7766);
#6704=AXIS2_PLACEMENT_3D('',#10008,#7767,#7768);
#6705=AXIS2_PLACEMENT_3D('',#10009,#7769,#7770);
#6706=AXIS2_PLACEMENT_3D('',#10011,#7771,#7772);
#6707=AXIS2_PLACEMENT_3D('',#10013,#7774,#7775);
#6708=AXIS2_PLACEMENT_3D('',#10014,#7776,#7777);
#6709=AXIS2_PLACEMENT_3D('',#10016,#7778,#7779);
#6710=AXIS2_PLACEMENT_3D('',#10018,#7780,#7781);
#6711=AXIS2_PLACEMENT_3D('',#10019,#7782,#7783);
#6712=AXIS2_PLACEMENT_3D('',#10021,#7785,#7786);
#6713=AXIS2_PLACEMENT_3D('',#10024,#7788,#7789);
#6714=AXIS2_PLACEMENT_3D('',#10025,#7790,#7791);
#6715=AXIS2_PLACEMENT_3D('',#10026,#7792,#7793);
#6716=AXIS2_PLACEMENT_3D('',#10027,#7794,#7795);
#6717=AXIS2_PLACEMENT_3D('',#10029,#7796,#7797);
#6718=AXIS2_PLACEMENT_3D('',#10032,#7799,#7800);
#6719=AXIS2_PLACEMENT_3D('',#10033,#7801,#7802);
#6720=AXIS2_PLACEMENT_3D('',#10035,#7803,#7804);
#6721=AXIS2_PLACEMENT_3D('',#10038,#7806,#7807);
#6722=AXIS2_PLACEMENT_3D('',#10039,#7808,#7809);
#6723=AXIS2_PLACEMENT_3D('',#10040,#7810,#7811);
#6724=AXIS2_PLACEMENT_3D('',#10041,#7812,#7813);
#6725=AXIS2_PLACEMENT_3D('',#10042,#7814,#7815);
#6726=AXIS2_PLACEMENT_3D('',#10044,#7816,#7817);
#6727=AXIS2_PLACEMENT_3D('',#10047,#7819,#7820);
#6728=AXIS2_PLACEMENT_3D('',#10048,#7821,#7822);
#6729=AXIS2_PLACEMENT_3D('',#10050,#7823,#7824);
#6730=AXIS2_PLACEMENT_3D('',#10053,#7826,#7827);
#6731=AXIS2_PLACEMENT_3D('',#10054,#7828,#7829);
#6732=AXIS2_PLACEMENT_3D('',#10055,#7830,#7831);
#6733=AXIS2_PLACEMENT_3D('',#10056,#7832,#7833);
#6734=AXIS2_PLACEMENT_3D('',#10057,#7834,#7835);
#6735=AXIS2_PLACEMENT_3D('',#10059,#7836,#7837);
#6736=AXIS2_PLACEMENT_3D('',#10061,#7838,#7839);
#6737=AXIS2_PLACEMENT_3D('',#10062,#7840,#7841);
#6738=AXIS2_PLACEMENT_3D('',#10064,#7842,#7843);
#6739=AXIS2_PLACEMENT_3D('',#10066,#7845,#7846);
#6740=AXIS2_PLACEMENT_3D('',#10067,#7847,#7848);
#6741=AXIS2_PLACEMENT_3D('',#10069,#7849,#7850);
#6742=AXIS2_PLACEMENT_3D('',#10071,#7851,#7852);
#6743=AXIS2_PLACEMENT_3D('',#10072,#7853,#7854);
#6744=AXIS2_PLACEMENT_3D('',#10074,#7856,#7857);
#6745=AXIS2_PLACEMENT_3D('',#10077,#7859,#7860);
#6746=AXIS2_PLACEMENT_3D('',#10078,#7861,#7862);
#6747=AXIS2_PLACEMENT_3D('',#10079,#7863,#7864);
#6748=AXIS2_PLACEMENT_3D('',#10080,#7865,#7866);
#6749=AXIS2_PLACEMENT_3D('',#10082,#7867,#7868);
#6750=AXIS2_PLACEMENT_3D('',#10085,#7870,#7871);
#6751=AXIS2_PLACEMENT_3D('',#10086,#7872,#7873);
#6752=AXIS2_PLACEMENT_3D('',#10088,#7874,#7875);
#6753=AXIS2_PLACEMENT_3D('',#10091,#7877,#7878);
#6754=AXIS2_PLACEMENT_3D('',#10092,#7879,#7880);
#6755=AXIS2_PLACEMENT_3D('',#10093,#7881,#7882);
#6756=AXIS2_PLACEMENT_3D('',#10094,#7883,#7884);
#6757=AXIS2_PLACEMENT_3D('',#10095,#7885,#7886);
#6758=AXIS2_PLACEMENT_3D('',#10097,#7887,#7888);
#6759=AXIS2_PLACEMENT_3D('',#10100,#7890,#7891);
#6760=AXIS2_PLACEMENT_3D('',#10101,#7892,#7893);
#6761=AXIS2_PLACEMENT_3D('',#10103,#7894,#7895);
#6762=AXIS2_PLACEMENT_3D('',#10106,#7897,#7898);
#6763=AXIS2_PLACEMENT_3D('',#10107,#7899,#7900);
#6764=AXIS2_PLACEMENT_3D('',#10108,#7901,#7902);
#6765=AXIS2_PLACEMENT_3D('',#10109,#7903,#7904);
#6766=AXIS2_PLACEMENT_3D('',#10110,#7905,#7906);
#6767=AXIS2_PLACEMENT_3D('',#10112,#7907,#7908);
#6768=AXIS2_PLACEMENT_3D('',#10114,#7909,#7910);
#6769=AXIS2_PLACEMENT_3D('',#10115,#7911,#7912);
#6770=AXIS2_PLACEMENT_3D('',#10117,#7913,#7914);
#6771=AXIS2_PLACEMENT_3D('',#10119,#7916,#7917);
#6772=AXIS2_PLACEMENT_3D('',#10120,#7918,#7919);
#6773=AXIS2_PLACEMENT_3D('',#10122,#7920,#7921);
#6774=AXIS2_PLACEMENT_3D('',#10124,#7922,#7923);
#6775=AXIS2_PLACEMENT_3D('',#10125,#7924,#7925);
#6776=AXIS2_PLACEMENT_3D('',#10127,#7927,#7928);
#6777=AXIS2_PLACEMENT_3D('',#10130,#7930,#7931);
#6778=AXIS2_PLACEMENT_3D('',#10131,#7932,#7933);
#6779=AXIS2_PLACEMENT_3D('',#10132,#7934,#7935);
#6780=AXIS2_PLACEMENT_3D('',#10133,#7936,#7937);
#6781=AXIS2_PLACEMENT_3D('',#10135,#7938,#7939);
#6782=AXIS2_PLACEMENT_3D('',#10138,#7941,#7942);
#6783=AXIS2_PLACEMENT_3D('',#10139,#7943,#7944);
#6784=AXIS2_PLACEMENT_3D('',#10141,#7945,#7946);
#6785=AXIS2_PLACEMENT_3D('',#10144,#7948,#7949);
#6786=AXIS2_PLACEMENT_3D('',#10145,#7950,#7951);
#6787=AXIS2_PLACEMENT_3D('',#10146,#7952,#7953);
#6788=AXIS2_PLACEMENT_3D('',#10147,#7954,#7955);
#6789=AXIS2_PLACEMENT_3D('',#10148,#7956,#7957);
#6790=AXIS2_PLACEMENT_3D('',#10150,#7958,#7959);
#6791=AXIS2_PLACEMENT_3D('',#10153,#7961,#7962);
#6792=AXIS2_PLACEMENT_3D('',#10154,#7963,#7964);
#6793=AXIS2_PLACEMENT_3D('',#10156,#7965,#7966);
#6794=AXIS2_PLACEMENT_3D('',#10159,#7968,#7969);
#6795=AXIS2_PLACEMENT_3D('',#10160,#7970,#7971);
#6796=AXIS2_PLACEMENT_3D('',#10161,#7972,#7973);
#6797=AXIS2_PLACEMENT_3D('',#10162,#7974,#7975);
#6798=AXIS2_PLACEMENT_3D('',#10163,#7976,#7977);
#6799=AXIS2_PLACEMENT_3D('',#10165,#7978,#7979);
#6800=AXIS2_PLACEMENT_3D('',#10167,#7980,#7981);
#6801=AXIS2_PLACEMENT_3D('',#10168,#7982,#7983);
#6802=AXIS2_PLACEMENT_3D('',#10170,#7984,#7985);
#6803=AXIS2_PLACEMENT_3D('',#10172,#7987,#7988);
#6804=AXIS2_PLACEMENT_3D('',#10173,#7989,#7990);
#6805=AXIS2_PLACEMENT_3D('',#10175,#7991,#7992);
#6806=AXIS2_PLACEMENT_3D('',#10177,#7993,#7994);
#6807=AXIS2_PLACEMENT_3D('',#10178,#7995,#7996);
#6808=AXIS2_PLACEMENT_3D('',#10180,#7998,#7999);
#6809=AXIS2_PLACEMENT_3D('',#10183,#8001,#8002);
#6810=AXIS2_PLACEMENT_3D('',#10184,#8003,#8004);
#6811=AXIS2_PLACEMENT_3D('',#10185,#8005,#8006);
#6812=AXIS2_PLACEMENT_3D('',#10186,#8007,#8008);
#6813=AXIS2_PLACEMENT_3D('',#10188,#8009,#8010);
#6814=AXIS2_PLACEMENT_3D('',#10191,#8012,#8013);
#6815=AXIS2_PLACEMENT_3D('',#10192,#8014,#8015);
#6816=AXIS2_PLACEMENT_3D('',#10194,#8016,#8017);
#6817=AXIS2_PLACEMENT_3D('',#10197,#8019,#8020);
#6818=AXIS2_PLACEMENT_3D('',#10198,#8021,#8022);
#6819=AXIS2_PLACEMENT_3D('',#10199,#8023,#8024);
#6820=AXIS2_PLACEMENT_3D('',#10200,#8025,#8026);
#6821=AXIS2_PLACEMENT_3D('',#10201,#8027,#8028);
#6822=AXIS2_PLACEMENT_3D('',#10203,#8029,#8030);
#6823=AXIS2_PLACEMENT_3D('',#10206,#8032,#8033);
#6824=AXIS2_PLACEMENT_3D('',#10207,#8034,#8035);
#6825=AXIS2_PLACEMENT_3D('',#10208,#8036,#8037);
#6826=AXIS2_PLACEMENT_3D('',#10209,#8038,#8039);
#6827=AXIS2_PLACEMENT_3D('',#10210,#8040,#8041);
#6828=AXIS2_PLACEMENT_3D('',#10212,#8042,#8043);
#6829=AXIS2_PLACEMENT_3D('',#10215,#8045,#8046);
#6830=AXIS2_PLACEMENT_3D('',#10216,#8047,#8048);
#6831=AXIS2_PLACEMENT_3D('',#10217,#8049,#8050);
#6832=AXIS2_PLACEMENT_3D('',#10218,#8051,#8052);
#6833=AXIS2_PLACEMENT_3D('',#10219,#8053,#8054);
#6834=AXIS2_PLACEMENT_3D('',#10221,#8055,#8056);
#6835=AXIS2_PLACEMENT_3D('',#10224,#8058,#8059);
#6836=AXIS2_PLACEMENT_3D('',#10225,#8060,#8061);
#6837=AXIS2_PLACEMENT_3D('',#10226,#8062,#8063);
#6838=AXIS2_PLACEMENT_3D('',#10228,#8064,#8065);
#6839=AXIS2_PLACEMENT_3D('',#10231,#8067,#8068);
#6840=AXIS2_PLACEMENT_3D('',#10232,#8069,#8070);
#6841=AXIS2_PLACEMENT_3D('',#10233,#8071,#8072);
#6842=AXIS2_PLACEMENT_3D('',#10235,#8073,#8074);
#6843=AXIS2_PLACEMENT_3D('',#10238,#8076,#8077);
#6844=AXIS2_PLACEMENT_3D('',#10239,#8078,#8079);
#6845=AXIS2_PLACEMENT_3D('',#10240,#8080,#8081);
#6846=AXIS2_PLACEMENT_3D('',#10242,#8082,#8083);
#6847=AXIS2_PLACEMENT_3D('',#10245,#8085,#8086);
#6848=AXIS2_PLACEMENT_3D('',#10246,#8087,#8088);
#6849=AXIS2_PLACEMENT_3D('',#10247,#8089,#8090);
#6850=AXIS2_PLACEMENT_3D('',#10249,#8091,#8092);
#6851=AXIS2_PLACEMENT_3D('',#10286,#8094,#8095);
#6852=AXIS2_PLACEMENT_3D('',#10288,#8096,#8097);
#6853=AXIS2_PLACEMENT_3D('',#10325,#8099,#8100);
#6854=AXIS2_PLACEMENT_3D('',#10327,#8101,#8102);
#6855=AXIS2_PLACEMENT_3D('',#10364,#8104,#8105);
#6856=AXIS2_PLACEMENT_3D('',#10366,#8106,#8107);
#6857=AXIS2_PLACEMENT_3D('',#10403,#8109,#8110);
#6858=AXIS2_PLACEMENT_3D('',#10412,#8115,#8116);
#6859=AXIS2_PLACEMENT_3D('',#10415,#8117,#8118);
#6860=AXIS2_PLACEMENT_3D('',#10419,#8121,#8122);
#6861=AXIS2_PLACEMENT_3D('',#10422,#8123,#8124);
#6862=AXIS2_PLACEMENT_3D('',#10426,#8127,#8128);
#6863=AXIS2_PLACEMENT_3D('',#10427,#8129,#8130);
#6864=AXIS2_PLACEMENT_3D('',#10429,#8132,#8133);
#6865=AXIS2_PLACEMENT_3D('',#10432,#8136,#8137);
#6866=AXIS2_PLACEMENT_3D('',#10433,#8138,#8139);
#6867=AXIS2_PLACEMENT_3D('',#10435,#8141,#8142);
#6868=AXIS2_PLACEMENT_3D('',#10445,#8148,#8149);
#6869=AXIS2_PLACEMENT_3D('',#10451,#8153,#8154);
#6870=AXIS2_PLACEMENT_3D('',#10453,#8155,#8156);
#6871=AXIS2_PLACEMENT_3D('',#10457,#8159,#8160);
#6872=AXIS2_PLACEMENT_3D('',#10463,#8164,#8165);
#6873=AXIS2_PLACEMENT_3D('',#10464,#8166,#8167);
#6874=AXIS2_PLACEMENT_3D('',#10466,#8169,#8170);
#6875=AXIS2_PLACEMENT_3D('',#10469,#8173,#8174);
#6876=AXIS2_PLACEMENT_3D('',#10471,#8175,#8176);
#6877=AXIS2_PLACEMENT_3D('',#10474,#8178,#8179);
#6878=AXIS2_PLACEMENT_3D('',#10475,#8180,#8181);
#6879=AXIS2_PLACEMENT_3D('',#10477,#8182,#8183);
#6880=AXIS2_PLACEMENT_3D('',#10481,#8186,#8187);
#6881=AXIS2_PLACEMENT_3D('',#10482,#8188,#8189);
#6882=AXIS2_PLACEMENT_3D('',#10483,#8190,#8191);
#6883=AXIS2_PLACEMENT_3D('',#10485,#8192,#8193);
#6884=AXIS2_PLACEMENT_3D('',#10488,#8195,#8196);
#6885=AXIS2_PLACEMENT_3D('',#10489,#8197,#8198);
#6886=AXIS2_PLACEMENT_3D('',#10490,#8199,#8200);
#6887=AXIS2_PLACEMENT_3D('',#10491,#8201,#8202);
#6888=AXIS2_PLACEMENT_3D('',#10492,#8203,#8204);
#6889=AXIS2_PLACEMENT_3D('',#10494,#8205,#8206);
#6890=AXIS2_PLACEMENT_3D('',#10497,#8208,#8209);
#6891=AXIS2_PLACEMENT_3D('',#10498,#8210,#8211);
#6892=AXIS2_PLACEMENT_3D('',#10500,#8212,#8213);
#6893=AXIS2_PLACEMENT_3D('',#10503,#8215,#8216);
#6894=AXIS2_PLACEMENT_3D('',#10504,#8217,#8218);
#6895=AXIS2_PLACEMENT_3D('',#10506,#8219,#8220);
#6896=AXIS2_PLACEMENT_3D('',#10509,#8222,#8223);
#6897=AXIS2_PLACEMENT_3D('',#10510,#8224,#8225);
#6898=AXIS2_PLACEMENT_3D('',#10512,#8226,#8227);
#6899=AXIS2_PLACEMENT_3D('',#10515,#8229,#8230);
#6900=AXIS2_PLACEMENT_3D('',#10516,#8231,#8232);
#6901=AXIS2_PLACEMENT_3D('',#10525,#8237,#8238);
#6902=AXIS2_PLACEMENT_3D('',#10531,#8242,#8243);
#6903=AXIS2_PLACEMENT_3D('',#10537,#8247,#8248);
#6904=AXIS2_PLACEMENT_3D('',#10540,#8251,#8252);
#6905=AXIS2_PLACEMENT_3D('',#10549,#8257,#8258);
#6906=AXIS2_PLACEMENT_3D('',#10555,#8262,#8263);
#6907=AXIS2_PLACEMENT_3D('',#10561,#8267,#8268);
#6908=AXIS2_PLACEMENT_3D('',#10564,#8271,#8272);
#6909=AXIS2_PLACEMENT_3D('',#10565,#8273,#8274);
#6910=AXIS2_PLACEMENT_3D('',#10566,#8275,#8276);
#6911=AXIS2_PLACEMENT_3D('',#10567,#8277,#8278);
#6912=AXIS2_PLACEMENT_3D('',#10569,#8279,#8280);
#6913=AXIS2_PLACEMENT_3D('',#10572,#8282,#8283);
#6914=AXIS2_PLACEMENT_3D('',#10573,#8284,#8285);
#6915=AXIS2_PLACEMENT_3D('',#10575,#8286,#8287);
#6916=AXIS2_PLACEMENT_3D('',#10578,#8289,#8290);
#6917=AXIS2_PLACEMENT_3D('',#10579,#8291,#8292);
#6918=AXIS2_PLACEMENT_3D('',#10581,#8293,#8294);
#6919=AXIS2_PLACEMENT_3D('',#10584,#8296,#8297);
#6920=AXIS2_PLACEMENT_3D('',#10585,#8298,#8299);
#6921=AXIS2_PLACEMENT_3D('',#10587,#8300,#8301);
#6922=AXIS2_PLACEMENT_3D('',#10590,#8303,#8304);
#6923=AXIS2_PLACEMENT_3D('',#10591,#8305,#8306);
#6924=AXIS2_PLACEMENT_3D('',#10600,#8311,#8312);
#6925=AXIS2_PLACEMENT_3D('',#10606,#8316,#8317);
#6926=AXIS2_PLACEMENT_3D('',#10612,#8321,#8322);
#6927=AXIS2_PLACEMENT_3D('',#10615,#8325,#8326);
#6928=AXIS2_PLACEMENT_3D('',#10616,#8327,#8328);
#6929=AXIS2_PLACEMENT_3D('',#10617,#8329,#8330);
#6930=AXIS2_PLACEMENT_3D('',#10618,#8331,#8332);
#6931=AXIS2_PLACEMENT_3D('',#10620,#8333,#8334);
#6932=AXIS2_PLACEMENT_3D('',#10623,#8336,#8337);
#6933=AXIS2_PLACEMENT_3D('',#10624,#8338,#8339);
#6934=AXIS2_PLACEMENT_3D('',#10626,#8340,#8341);
#6935=AXIS2_PLACEMENT_3D('',#10629,#8343,#8344);
#6936=AXIS2_PLACEMENT_3D('',#10630,#8345,#8346);
#6937=AXIS2_PLACEMENT_3D('',#10632,#8347,#8348);
#6938=AXIS2_PLACEMENT_3D('',#10635,#8350,#8351);
#6939=AXIS2_PLACEMENT_3D('',#10636,#8352,#8353);
#6940=AXIS2_PLACEMENT_3D('',#10638,#8354,#8355);
#6941=AXIS2_PLACEMENT_3D('',#10641,#8357,#8358);
#6942=AXIS2_PLACEMENT_3D('',#10642,#8359,#8360);
#6943=AXIS2_PLACEMENT_3D('',#10651,#8365,#8366);
#6944=AXIS2_PLACEMENT_3D('',#10657,#8370,#8371);
#6945=AXIS2_PLACEMENT_3D('',#10663,#8375,#8376);
#6946=AXIS2_PLACEMENT_3D('',#10666,#8379,#8380);
#6947=AXIS2_PLACEMENT_3D('',#10675,#8385,#8386);
#6948=AXIS2_PLACEMENT_3D('',#10681,#8390,#8391);
#6949=AXIS2_PLACEMENT_3D('',#10687,#8395,#8396);
#6950=AXIS2_PLACEMENT_3D('',#10690,#8399,#8400);
#6951=AXIS2_PLACEMENT_3D('',#10691,#8401,#8402);
#6952=AXIS2_PLACEMENT_3D('',#10692,#8403,#8404);
#6953=AXIS2_PLACEMENT_3D('',#10693,#8405,#8406);
#6954=AXIS2_PLACEMENT_3D('',#10702,#8411,#8412);
#6955=AXIS2_PLACEMENT_3D('',#10711,#8417,#8418);
#6956=AXIS2_PLACEMENT_3D('',#10712,#8419,#8420);
#6957=AXIS2_PLACEMENT_3D('',#10713,#8421,#8422);
#6958=AXIS2_PLACEMENT_3D('',#10714,#8423,#8424);
#6959=AXIS2_PLACEMENT_3D('',#10715,#8425,#8426);
#6960=AXIS2_PLACEMENT_3D('',#10716,#8427,#8428);
#6961=AXIS2_PLACEMENT_3D('',#10718,#8429,#8430);
#6962=AXIS2_PLACEMENT_3D('',#10719,#8431,#8432);
#6963=AXIS2_PLACEMENT_3D('',#10720,#8433,#8434);
#6964=AXIS2_PLACEMENT_3D('',#10722,#8435,#8436);
#6965=AXIS2_PLACEMENT_3D('',#10724,#8437,#8438);
#6966=AXIS2_PLACEMENT_3D('',#10725,#8439,#8440);
#6967=AXIS2_PLACEMENT_3D('',#10727,#8442,#8443);
#6968=AXIS2_PLACEMENT_3D('',#10729,#8444,#8445);
#6969=AXIS2_PLACEMENT_3D('',#10731,#8447,#8448);
#6970=AXIS2_PLACEMENT_3D('',#10732,#8449,#8450);
#6971=AXIS2_PLACEMENT_3D('',#10733,#8451,#8452);
#6972=AXIS2_PLACEMENT_3D('',#10742,#8457,#8458);
#6973=AXIS2_PLACEMENT_3D('',#10751,#8463,#8464);
#6974=AXIS2_PLACEMENT_3D('',#10752,#8465,#8466);
#6975=AXIS2_PLACEMENT_3D('',#10753,#8467,#8468);
#6976=AXIS2_PLACEMENT_3D('',#10754,#8469,#8470);
#6977=AXIS2_PLACEMENT_3D('',#10755,#8471,#8472);
#6978=AXIS2_PLACEMENT_3D('',#10756,#8473,#8474);
#6979=AXIS2_PLACEMENT_3D('',#10758,#8475,#8476);
#6980=AXIS2_PLACEMENT_3D('',#10759,#8477,#8478);
#6981=AXIS2_PLACEMENT_3D('',#10760,#8479,#8480);
#6982=AXIS2_PLACEMENT_3D('',#10762,#8481,#8482);
#6983=AXIS2_PLACEMENT_3D('',#10764,#8483,#8484);
#6984=AXIS2_PLACEMENT_3D('',#10765,#8485,#8486);
#6985=AXIS2_PLACEMENT_3D('',#10767,#8488,#8489);
#6986=AXIS2_PLACEMENT_3D('',#10769,#8490,#8491);
#6987=AXIS2_PLACEMENT_3D('',#10771,#8493,#8494);
#6988=AXIS2_PLACEMENT_3D('',#10772,#8495,#8496);
#6989=AXIS2_PLACEMENT_3D('',#10773,#8497,#8498);
#6990=AXIS2_PLACEMENT_3D('',#10782,#8503,#8504);
#6991=AXIS2_PLACEMENT_3D('',#10791,#8509,#8510);
#6992=AXIS2_PLACEMENT_3D('',#10792,#8511,#8512);
#6993=AXIS2_PLACEMENT_3D('',#10793,#8513,#8514);
#6994=AXIS2_PLACEMENT_3D('',#10794,#8515,#8516);
#6995=AXIS2_PLACEMENT_3D('',#10795,#8517,#8518);
#6996=AXIS2_PLACEMENT_3D('',#10796,#8519,#8520);
#6997=AXIS2_PLACEMENT_3D('',#10798,#8521,#8522);
#6998=AXIS2_PLACEMENT_3D('',#10799,#8523,#8524);
#6999=AXIS2_PLACEMENT_3D('',#10800,#8525,#8526);
#7000=AXIS2_PLACEMENT_3D('',#10802,#8527,#8528);
#7001=AXIS2_PLACEMENT_3D('',#10804,#8529,#8530);
#7002=AXIS2_PLACEMENT_3D('',#10805,#8531,#8532);
#7003=AXIS2_PLACEMENT_3D('',#10807,#8534,#8535);
#7004=AXIS2_PLACEMENT_3D('',#10809,#8536,#8537);
#7005=AXIS2_PLACEMENT_3D('',#10811,#8539,#8540);
#7006=AXIS2_PLACEMENT_3D('',#10812,#8541,#8542);
#7007=AXIS2_PLACEMENT_3D('',#10813,#8543,#8544);
#7008=AXIS2_PLACEMENT_3D('',#10822,#8549,#8550);
#7009=AXIS2_PLACEMENT_3D('',#10831,#8555,#8556);
#7010=AXIS2_PLACEMENT_3D('',#10832,#8557,#8558);
#7011=AXIS2_PLACEMENT_3D('',#10833,#8559,#8560);
#7012=AXIS2_PLACEMENT_3D('',#10834,#8561,#8562);
#7013=AXIS2_PLACEMENT_3D('',#10835,#8563,#8564);
#7014=AXIS2_PLACEMENT_3D('',#10836,#8565,#8566);
#7015=AXIS2_PLACEMENT_3D('',#10838,#8567,#8568);
#7016=AXIS2_PLACEMENT_3D('',#10839,#8569,#8570);
#7017=AXIS2_PLACEMENT_3D('',#10840,#8571,#8572);
#7018=AXIS2_PLACEMENT_3D('',#10842,#8573,#8574);
#7019=AXIS2_PLACEMENT_3D('',#10844,#8575,#8576);
#7020=AXIS2_PLACEMENT_3D('',#10845,#8577,#8578);
#7021=AXIS2_PLACEMENT_3D('',#10847,#8580,#8581);
#7022=AXIS2_PLACEMENT_3D('',#10849,#8582,#8583);
#7023=AXIS2_PLACEMENT_3D('',#10851,#8585,#8586);
#7024=AXIS2_PLACEMENT_3D('',#10852,#8587,#8588);
#7025=AXIS2_PLACEMENT_3D('',#10853,#8589,#8590);
#7026=AXIS2_PLACEMENT_3D('',#10855,#8591,#8592);
#7027=AXIS2_PLACEMENT_3D('',#10858,#8594,#8595);
#7028=AXIS2_PLACEMENT_3D('',#10859,#8596,#8597);
#7029=AXIS2_PLACEMENT_3D('',#10861,#8598,#8599);
#7030=AXIS2_PLACEMENT_3D('',#10864,#8601,#8602);
#7031=AXIS2_PLACEMENT_3D('',#10865,#8603,#8604);
#7032=AXIS2_PLACEMENT_3D('',#10867,#8605,#8606);
#7033=AXIS2_PLACEMENT_3D('',#10870,#8608,#8609);
#7034=AXIS2_PLACEMENT_3D('',#10871,#8610,#8611);
#7035=AXIS2_PLACEMENT_3D('',#10873,#8612,#8613);
#7036=AXIS2_PLACEMENT_3D('',#10876,#8615,#8616);
#7037=AXIS2_PLACEMENT_3D('',#10877,#8617,#8618);
#7038=AXIS2_PLACEMENT_3D('',#10879,#8619,#8620);
#7039=AXIS2_PLACEMENT_3D('',#10882,#8622,#8623);
#7040=AXIS2_PLACEMENT_3D('',#10883,#8624,#8625);
#7041=AXIS2_PLACEMENT_3D('',#10885,#8626,#8627);
#7042=AXIS2_PLACEMENT_3D('',#10888,#8629,#8630);
#7043=AXIS2_PLACEMENT_3D('',#10889,#8631,#8632);
#7044=AXIS2_PLACEMENT_3D('',#10890,#8633,#8634);
#7045=AXIS2_PLACEMENT_3D('',#10891,#8635,#8636);
#7046=AXIS2_PLACEMENT_3D('',#10892,#8637,#8638);
#7047=AXIS2_PLACEMENT_3D('',#10894,#8639,#8640);
#7048=AXIS2_PLACEMENT_3D('',#10897,#8642,#8643);
#7049=AXIS2_PLACEMENT_3D('',#10898,#8644,#8645);
#7050=AXIS2_PLACEMENT_3D('',#10900,#8646,#8647);
#7051=AXIS2_PLACEMENT_3D('',#10903,#8649,#8650);
#7052=AXIS2_PLACEMENT_3D('',#10904,#8651,#8652);
#7053=AXIS2_PLACEMENT_3D('',#10906,#8653,#8654);
#7054=AXIS2_PLACEMENT_3D('',#10909,#8656,#8657);
#7055=AXIS2_PLACEMENT_3D('',#10910,#8658,#8659);
#7056=AXIS2_PLACEMENT_3D('',#10912,#8660,#8661);
#7057=AXIS2_PLACEMENT_3D('',#10915,#8663,#8664);
#7058=AXIS2_PLACEMENT_3D('',#10916,#8665,#8666);
#7059=AXIS2_PLACEMENT_3D('',#10918,#8667,#8668);
#7060=AXIS2_PLACEMENT_3D('',#10921,#8670,#8671);
#7061=AXIS2_PLACEMENT_3D('',#10922,#8672,#8673);
#7062=AXIS2_PLACEMENT_3D('',#10924,#8674,#8675);
#7063=AXIS2_PLACEMENT_3D('',#10927,#8677,#8678);
#7064=AXIS2_PLACEMENT_3D('',#10928,#8679,#8680);
#7065=AXIS2_PLACEMENT_3D('',#10929,#8681,#8682);
#7066=AXIS2_PLACEMENT_3D('',#10930,#8683,#8684);
#7067=AXIS2_PLACEMENT_3D('',#10931,#8685,#8686);
#7068=AXIS2_PLACEMENT_3D('',#10933,#8687,#8688);
#7069=AXIS2_PLACEMENT_3D('',#10936,#8690,#8691);
#7070=AXIS2_PLACEMENT_3D('',#10937,#8692,#8693);
#7071=AXIS2_PLACEMENT_3D('',#10939,#8694,#8695);
#7072=AXIS2_PLACEMENT_3D('',#10941,#8696,#8697);
#7073=AXIS2_PLACEMENT_3D('',#10942,#8698,#8699);
#7074=AXIS2_PLACEMENT_3D('',#10944,#8700,#8701);
#7075=AXIS2_PLACEMENT_3D('',#10946,#8703,#8704);
#7076=AXIS2_PLACEMENT_3D('',#10947,#8705,#8706);
#7077=AXIS2_PLACEMENT_3D('',#10950,#8708,#8709);
#7078=AXIS2_PLACEMENT_3D('',#10951,#8710,#8711);
#7079=AXIS2_PLACEMENT_3D('',#10952,#8712,#8713);
#7080=AXIS2_PLACEMENT_3D('',#10953,#8714,#8715);
#7081=AXIS2_PLACEMENT_3D('',#10962,#8720,#8721);
#7082=AXIS2_PLACEMENT_3D('',#10968,#8725,#8726);
#7083=AXIS2_PLACEMENT_3D('',#10974,#8730,#8731);
#7084=AXIS2_PLACEMENT_3D('',#10977,#8734,#8735);
#7085=AXIS2_PLACEMENT_3D('',#10978,#8736,#8737);
#7086=AXIS2_PLACEMENT_3D('',#10979,#8738,#8739);
#7087=AXIS2_PLACEMENT_3D('',#10980,#8740,#8741);
#7088=AXIS2_PLACEMENT_3D('',#10989,#8746,#8747);
#7089=AXIS2_PLACEMENT_3D('',#10995,#8751,#8752);
#7090=AXIS2_PLACEMENT_3D('',#11001,#8756,#8757);
#7091=AXIS2_PLACEMENT_3D('',#11004,#8760,#8761);
#7092=AXIS2_PLACEMENT_3D('',#11005,#8762,#8763);
#7093=AXIS2_PLACEMENT_3D('',#11006,#8764,#8765);
#7094=AXIS2_PLACEMENT_3D('',#11007,#8766,#8767);
#7095=AXIS2_PLACEMENT_3D('',#11016,#8772,#8773);
#7096=AXIS2_PLACEMENT_3D('',#11022,#8777,#8778);
#7097=AXIS2_PLACEMENT_3D('',#11028,#8782,#8783);
#7098=AXIS2_PLACEMENT_3D('',#11034,#8787,#8788);
#7099=AXIS2_PLACEMENT_3D('',#11040,#8792,#8793);
#7100=AXIS2_PLACEMENT_3D('',#11043,#8796,#8797);
#7101=AXIS2_PLACEMENT_3D('',#11044,#8798,#8799);
#7102=AXIS2_PLACEMENT_3D('',#11045,#8800,#8801);
#7103=AXIS2_PLACEMENT_3D('',#11047,#8802,#8803);
#7104=AXIS2_PLACEMENT_3D('',#11048,#8804,#8805);
#7105=AXIS2_PLACEMENT_3D('',#11050,#8806,#8807);
#7106=AXIS2_PLACEMENT_3D('',#11051,#8808,#8809);
#7107=AXIS2_PLACEMENT_3D('',#11053,#8810,#8811);
#7108=AXIS2_PLACEMENT_3D('',#11055,#8813,#8814);
#7109=AXIS2_PLACEMENT_3D('',#11057,#8815,#8816);
#7110=AXIS2_PLACEMENT_3D('',#11059,#8818,#8819);
#7111=AXIS2_PLACEMENT_3D('',#11061,#8820,#8821);
#7112=AXIS2_PLACEMENT_3D('',#11063,#8823,#8824);
#7113=AXIS2_PLACEMENT_3D('',#11065,#8825,#8826);
#7114=AXIS2_PLACEMENT_3D('',#11066,#8827,#8828);
#7115=AXIS2_PLACEMENT_3D('',#11068,#8829,#8830);
#7116=AXIS2_PLACEMENT_3D('',#11070,#8832,#8833);
#7117=AXIS2_PLACEMENT_3D('',#11072,#8835,#8836);
#7118=AXIS2_PLACEMENT_3D('',#11073,#8837,#8838);
#7119=AXIS2_PLACEMENT_3D('',#11074,#8839,#8840);
#7120=AXIS2_PLACEMENT_3D('',#11076,#8841,#8842);
#7121=AXIS2_PLACEMENT_3D('',#11079,#8844,#8845);
#7122=AXIS2_PLACEMENT_3D('',#11080,#8846,#8847);
#7123=AXIS2_PLACEMENT_3D('',#11082,#8848,#8849);
#7124=AXIS2_PLACEMENT_3D('',#11083,#8850,#8851);
#7125=AXIS2_PLACEMENT_3D('',#11097,#8858,#8859);
#7126=AXIS2_PLACEMENT_3D('',#11098,#8860,#8861);
#7127=AXIS2_PLACEMENT_3D('',#11112,#8868,#8869);
#7128=AXIS2_PLACEMENT_3D('',#11113,#8870,#8871);
#7129=AXIS2_PLACEMENT_3D('',#11116,#8874,#8875);
#7130=AXIS2_PLACEMENT_3D('',#11118,#8877,#8878);
#7131=AXIS2_PLACEMENT_3D('',#11120,#8880,#8881);
#7132=AXIS2_PLACEMENT_3D('',#11122,#8883,#8884);
#7133=AXIS2_PLACEMENT_3D('',#11124,#8886,#8887);
#7134=AXIS2_PLACEMENT_3D('',#11125,#8888,#8889);
#7135=AXIS2_PLACEMENT_3D('',#11127,#8890,#8891);
#7136=AXIS2_PLACEMENT_3D('',#11128,#8892,#8893);
#7137=AXIS2_PLACEMENT_3D('',#11131,#8895,#8896);
#7138=AXIS2_PLACEMENT_3D('',#11132,#8897,#8898);
#7139=AXIS2_PLACEMENT_3D('',#11134,#8899,#8900);
#7140=AXIS2_PLACEMENT_3D('',#11135,#8901,#8902);
#7141=AXIS2_PLACEMENT_3D('',#11137,#8904,#8905);
#7142=AXIS2_PLACEMENT_3D('',#11139,#8906,#8907);
#7143=AXIS2_PLACEMENT_3D('',#11141,#8909,#8910);
#7144=AXIS2_PLACEMENT_3D('',#11143,#8911,#8912);
#7145=AXIS2_PLACEMENT_3D('',#11144,#8913,#8914);
#7146=AXIS2_PLACEMENT_3D('',#11146,#8916,#8917);
#7147=AXIS2_PLACEMENT_3D('',#11147,#8918,#8919);
#7148=AXIS2_PLACEMENT_3D('',#11149,#8920,#8921);
#7149=AXIS2_PLACEMENT_3D('',#11151,#8922,#8923);
#7150=AXIS2_PLACEMENT_3D('',#11152,#8924,#8925);
#7151=AXIS2_PLACEMENT_3D('',#11154,#8926,#8927);
#7152=AXIS2_PLACEMENT_3D('',#11156,#8929,#8930);
#7153=AXIS2_PLACEMENT_3D('',#11158,#8931,#8932);
#7154=AXIS2_PLACEMENT_3D('',#11159,#8933,#8934);
#7155=AXIS2_PLACEMENT_3D('',#11161,#8935,#8936);
#7156=AXIS2_PLACEMENT_3D('',#11163,#8938,#8939);
#7157=AXIS2_PLACEMENT_3D('',#11165,#8940,#8941);
#7158=AXIS2_PLACEMENT_3D('',#11166,#8942,#8943);
#7159=AXIS2_PLACEMENT_3D('',#11168,#8945,#8946);
#7160=AXIS2_PLACEMENT_3D('',#11169,#8947,#8948);
#7161=AXIS2_PLACEMENT_3D('',#11170,#8949,#8950);
#7162=AXIS2_PLACEMENT_3D('',#11171,#8951,#8952);
#7163=AXIS2_PLACEMENT_3D('',#11185,#8959,#8960);
#7164=AXIS2_PLACEMENT_3D('',#11186,#8961,#8962);
#7165=AXIS2_PLACEMENT_3D('',#11200,#8969,#8970);
#7166=AXIS2_PLACEMENT_3D('',#11201,#8971,#8972);
#7167=AXIS2_PLACEMENT_3D('',#11204,#8975,#8976);
#7168=AXIS2_PLACEMENT_3D('',#11206,#8978,#8979);
#7169=AXIS2_PLACEMENT_3D('',#11208,#8981,#8982);
#7170=AXIS2_PLACEMENT_3D('',#11210,#8984,#8985);
#7171=AXIS2_PLACEMENT_3D('',#11212,#8987,#8988);
#7172=AXIS2_PLACEMENT_3D('',#11213,#8989,#8990);
#7173=AXIS2_PLACEMENT_3D('',#11216,#8992,#8993);
#7174=AXIS2_PLACEMENT_3D('',#11217,#8994,#8995);
#7175=AXIS2_PLACEMENT_3D('',#11219,#8996,#8997);
#7176=AXIS2_PLACEMENT_3D('',#11221,#8998,#8999);
#7177=AXIS2_PLACEMENT_3D('',#11222,#9000,#9001);
#7178=AXIS2_PLACEMENT_3D('',#11224,#9003,#9004);
#7179=AXIS2_PLACEMENT_3D('',#11226,#9005,#9006);
#7180=AXIS2_PLACEMENT_3D('',#11228,#9008,#9009);
#7181=AXIS2_PLACEMENT_3D('',#11230,#9010,#9011);
#7182=AXIS2_PLACEMENT_3D('',#11232,#9013,#9014);
#7183=AXIS2_PLACEMENT_3D('',#11234,#9015,#9016);
#7184=AXIS2_PLACEMENT_3D('',#11235,#9017,#9018);
#7185=AXIS2_PLACEMENT_3D('',#11237,#9020,#9021);
#7186=AXIS2_PLACEMENT_3D('',#11238,#9022,#9023);
#7187=AXIS2_PLACEMENT_3D('',#11240,#9024,#9025);
#7188=AXIS2_PLACEMENT_3D('',#11241,#9026,#9027);
#7189=AXIS2_PLACEMENT_3D('',#11243,#9028,#9029);
#7190=AXIS2_PLACEMENT_3D('',#11245,#9031,#9032);
#7191=AXIS2_PLACEMENT_3D('',#11247,#9033,#9034);
#7192=AXIS2_PLACEMENT_3D('',#11249,#9036,#9037);
#7193=AXIS2_PLACEMENT_3D('',#11251,#9038,#9039);
#7194=AXIS2_PLACEMENT_3D('',#11253,#9041,#9042);
#7195=AXIS2_PLACEMENT_3D('',#11255,#9043,#9044);
#7196=AXIS2_PLACEMENT_3D('',#11256,#9045,#9046);
#7197=AXIS2_PLACEMENT_3D('',#11258,#9047,#9048);
#7198=AXIS2_PLACEMENT_3D('',#11260,#9050,#9051);
#7199=AXIS2_PLACEMENT_3D('',#11262,#9052,#9053);
#7200=AXIS2_PLACEMENT_3D('',#11264,#9055,#9056);
#7201=AXIS2_PLACEMENT_3D('',#11266,#9057,#9058);
#7202=AXIS2_PLACEMENT_3D('',#11268,#9060,#9061);
#7203=AXIS2_PLACEMENT_3D('',#11269,#9062,#9063);
#7204=AXIS2_PLACEMENT_3D('',#11278,#9068,#9069);
#7205=AXIS2_PLACEMENT_3D('',#11284,#9073,#9074);
#7206=AXIS2_PLACEMENT_3D('',#11290,#9078,#9079);
#7207=AXIS2_PLACEMENT_3D('',#11296,#9083,#9084);
#7208=AXIS2_PLACEMENT_3D('',#11302,#9088,#9089);
#7209=AXIS2_PLACEMENT_3D('',#11305,#9092,#9093);
#7210=AXIS2_PLACEMENT_3D('',#11306,#9094,#9095);
#7211=AXIS2_PLACEMENT_3D('',#11307,#9096,#9097);
#7212=AXIS2_PLACEMENT_3D('',#11308,#9098,#9099);
#7213=AXIS2_PLACEMENT_3D('',#11309,#9100,#9101);
#7214=AXIS2_PLACEMENT_3D('',#11310,#9102,#9103);
#7215=AXIS2_PLACEMENT_3D('',#11311,#9104,#9105);
#7216=AXIS2_PLACEMENT_3D('',#11312,#9106,#9107);
#7217=AXIS2_PLACEMENT_3D('',#11313,#9108,#9109);
#7218=AXIS2_PLACEMENT_3D('',#11314,#9110,#9111);
#7219=AXIS2_PLACEMENT_3D('',#11315,#9112,#9113);
#7220=AXIS2_PLACEMENT_3D('',#11316,#9114,#9115);
#7221=AXIS2_PLACEMENT_3D('',#11317,#9116,#9117);
#7222=AXIS2_PLACEMENT_3D('',#11318,#9118,#9119);
#7223=AXIS2_PLACEMENT_3D('',#11319,#9120,#9121);
#7224=AXIS2_PLACEMENT_3D('',#11320,#9122,#9123);
#7225=AXIS2_PLACEMENT_3D('',#11321,#9124,#9125);
#7226=AXIS2_PLACEMENT_3D('',#11322,#9126,#9127);
#7227=AXIS2_PLACEMENT_3D('',#11323,#9128,#9129);
#7228=AXIS2_PLACEMENT_3D('',#11324,#9130,#9131);
#7229=AXIS2_PLACEMENT_3D('',#11325,#9132,#9133);
#7230=AXIS2_PLACEMENT_3D('',#11326,#9134,#9135);
#7231=AXIS2_PLACEMENT_3D('',#11327,#9136,#9137);
#7232=AXIS2_PLACEMENT_3D('',#11328,#9138,#9139);
#7233=AXIS2_PLACEMENT_3D('',#11329,#9140,#9141);
#7234=AXIS2_PLACEMENT_3D('',#11330,#9142,#9143);
#7235=AXIS2_PLACEMENT_3D('',#11331,#9144,#9145);
#7236=AXIS2_PLACEMENT_3D('',#11332,#9146,#9147);
#7237=AXIS2_PLACEMENT_3D('',#11333,#9148,#9149);
#7238=AXIS2_PLACEMENT_3D('',#11334,#9150,#9151);
#7239=AXIS2_PLACEMENT_3D('',#11335,#9152,#9153);
#7240=AXIS2_PLACEMENT_3D('',#11336,#9154,#9155);
#7241=AXIS2_PLACEMENT_3D('',#11337,#9156,#9157);
#7242=AXIS2_PLACEMENT_3D('',#11338,#9158,#9159);
#7243=AXIS2_PLACEMENT_3D('',#11339,#9160,#9161);
#7244=AXIS2_PLACEMENT_3D('',#11340,#9162,#9163);
#7245=AXIS2_PLACEMENT_3D('',#11341,#9164,#9165);
#7246=AXIS2_PLACEMENT_3D('',#11342,#9166,#9167);
#7247=AXIS2_PLACEMENT_3D('',#11343,#9168,#9169);
#7248=AXIS2_PLACEMENT_3D('',#11344,#9170,#9171);
#7249=AXIS2_PLACEMENT_3D('',#11345,#9172,#9173);
#7250=AXIS2_PLACEMENT_3D('',#11346,#9174,#9175);
#7251=AXIS2_PLACEMENT_3D('',#11347,#9176,#9177);
#7252=AXIS2_PLACEMENT_3D('',#11348,#9178,#9179);
#7253=AXIS2_PLACEMENT_3D('',#11349,#9180,#9181);
#7254=AXIS2_PLACEMENT_3D('',#11350,#9182,#9183);
#7255=AXIS2_PLACEMENT_3D('',#11351,#9184,#9185);
#7256=AXIS2_PLACEMENT_3D('',#11352,#9186,#9187);
#7257=AXIS2_PLACEMENT_3D('',#11353,#9188,#9189);
#7258=AXIS2_PLACEMENT_3D('',#11354,#9190,#9191);
#7259=DIRECTION('axis',(0.,0.,1.));
#7260=DIRECTION('refdir',(1.,0.,0.));
#7261=DIRECTION('axis',(0.,0.,1.));
#7262=DIRECTION('refdir',(1.,0.,0.));
#7263=DIRECTION('center_axis',(0.,0.,1.));
#7264=DIRECTION('ref_axis',(1.,0.,0.));
#7265=DIRECTION('center_axis',(0.,0.,1.));
#7266=DIRECTION('ref_axis',(1.,0.,0.));
#7267=DIRECTION('',(0.,0.,1.));
#7268=DIRECTION('center_axis',(0.,0.,-1.));
#7269=DIRECTION('ref_axis',(1.,0.,0.));
#7270=DIRECTION('center_axis',(0.,0.,1.));
#7271=DIRECTION('ref_axis',(1.,0.,0.));
#7272=DIRECTION('center_axis',(0.,0.,1.));
#7273=DIRECTION('ref_axis',(1.,0.,0.));
#7274=DIRECTION('',(0.,0.,1.));
#7275=DIRECTION('center_axis',(0.,0.,-1.));
#7276=DIRECTION('ref_axis',(1.,0.,0.));
#7277=DIRECTION('center_axis',(0.,0.,1.));
#7278=DIRECTION('ref_axis',(1.,0.,0.));
#7279=DIRECTION('center_axis',(0.,0.,1.));
#7280=DIRECTION('ref_axis',(1.,0.,0.));
#7281=DIRECTION('',(0.,0.,1.));
#7282=DIRECTION('center_axis',(0.,0.,-1.));
#7283=DIRECTION('ref_axis',(1.,0.,0.));
#7284=DIRECTION('center_axis',(0.,0.,1.));
#7285=DIRECTION('ref_axis',(1.,0.,0.));
#7286=DIRECTION('center_axis',(0.,0.,1.));
#7287=DIRECTION('ref_axis',(1.,0.,0.));
#7288=DIRECTION('',(0.,0.,1.));
#7289=DIRECTION('center_axis',(0.,0.,-1.));
#7290=DIRECTION('ref_axis',(1.,0.,0.));
#7291=DIRECTION('center_axis',(0.,1.,0.));
#7292=DIRECTION('ref_axis',(-1.,0.,0.));
#7293=DIRECTION('',(-1.,0.,0.));
#7294=DIRECTION('',(0.,0.,1.));
#7295=DIRECTION('',(-1.,0.,0.));
#7296=DIRECTION('',(0.,0.,1.));
#7297=DIRECTION('center_axis',(1.,0.,0.));
#7298=DIRECTION('ref_axis',(0.,1.,0.));
#7299=DIRECTION('',(0.,1.,0.));
#7300=DIRECTION('',(0.,1.,0.));
#7301=DIRECTION('',(0.,0.,1.));
#7302=DIRECTION('center_axis',(0.,-1.,0.));
#7303=DIRECTION('ref_axis',(1.,0.,0.));
#7304=DIRECTION('',(1.,0.,0.));
#7305=DIRECTION('',(1.,0.,0.));
#7306=DIRECTION('',(0.,0.,1.));
#7307=DIRECTION('center_axis',(-1.,0.,0.));
#7308=DIRECTION('ref_axis',(0.,-1.,0.));
#7309=DIRECTION('',(0.,-1.,0.));
#7310=DIRECTION('',(0.,-1.,0.));
#7311=DIRECTION('center_axis',(0.,0.,1.));
#7312=DIRECTION('ref_axis',(1.,0.,0.));
#7313=DIRECTION('center_axis',(0.,0.,1.));
#7314=DIRECTION('ref_axis',(1.,0.,0.));
#7315=DIRECTION('axis',(0.,0.,1.));
#7316=DIRECTION('refdir',(1.,0.,0.));
#7317=DIRECTION('center_axis',(0.,0.,1.));
#7318=DIRECTION('ref_axis',(1.,0.,0.));
#7319=DIRECTION('center_axis',(0.,0.,1.));
#7320=DIRECTION('ref_axis',(1.,0.,0.));
#7321=DIRECTION('',(0.,0.,1.));
#7322=DIRECTION('center_axis',(0.,0.,-1.));
#7323=DIRECTION('ref_axis',(1.,0.,0.));
#7324=DIRECTION('center_axis',(0.,0.,1.));
#7325=DIRECTION('ref_axis',(1.,0.,0.));
#7326=DIRECTION('center_axis',(0.,0.,1.));
#7327=DIRECTION('ref_axis',(1.,0.,0.));
#7328=DIRECTION('center_axis',(0.,0.,1.));
#7329=DIRECTION('ref_axis',(1.,0.,0.));
#7330=DIRECTION('',(0.,0.,1.));
#7331=DIRECTION('center_axis',(0.,0.,-1.));
#7332=DIRECTION('ref_axis',(1.,0.,0.));
#7333=DIRECTION('center_axis',(0.,0.,1.));
#7334=DIRECTION('ref_axis',(1.,0.,0.));
#7335=DIRECTION('center_axis',(0.,0.,1.));
#7336=DIRECTION('ref_axis',(1.,0.,0.));
#7337=DIRECTION('center_axis',(0.,0.,1.));
#7338=DIRECTION('ref_axis',(1.,0.,0.));
#7339=DIRECTION('center_axis',(0.,0.,1.));
#7340=DIRECTION('ref_axis',(1.,0.,0.));
#7341=DIRECTION('',(0.,0.,1.));
#7342=DIRECTION('center_axis',(0.,0.,-1.));
#7343=DIRECTION('ref_axis',(1.,0.,0.));
#7344=DIRECTION('center_axis',(0.,0.,1.));
#7345=DIRECTION('ref_axis',(1.,0.,0.));
#7346=DIRECTION('center_axis',(0.,0.,1.));
#7347=DIRECTION('ref_axis',(1.,0.,0.));
#7348=DIRECTION('center_axis',(0.,0.,1.));
#7349=DIRECTION('ref_axis',(1.,0.,0.));
#7350=DIRECTION('center_axis',(0.,0.,1.));
#7351=DIRECTION('ref_axis',(1.,0.,0.));
#7352=DIRECTION('',(0.,0.,1.));
#7353=DIRECTION('center_axis',(0.,0.,1.));
#7354=DIRECTION('ref_axis',(1.,0.,0.));
#7355=DIRECTION('center_axis',(0.,0.,1.));
#7356=DIRECTION('ref_axis',(1.,0.,0.));
#7357=DIRECTION('',(0.,0.,1.));
#7358=DIRECTION('center_axis',(0.,1.,0.));
#7359=DIRECTION('ref_axis',(-1.,0.,0.));
#7360=DIRECTION('',(-1.,0.,0.));
#7361=DIRECTION('',(0.,0.,1.));
#7362=DIRECTION('',(-1.,0.,0.));
#7363=DIRECTION('',(0.,0.,1.));
#7364=DIRECTION('center_axis',(1.,0.,0.));
#7365=DIRECTION('ref_axis',(0.,1.,0.));
#7366=DIRECTION('',(0.,1.,0.));
#7367=DIRECTION('',(0.,1.,0.));
#7368=DIRECTION('',(0.,0.,1.));
#7369=DIRECTION('center_axis',(0.,-1.,0.));
#7370=DIRECTION('ref_axis',(1.,0.,0.));
#7371=DIRECTION('',(1.,0.,0.));
#7372=DIRECTION('',(1.,0.,0.));
#7373=DIRECTION('',(0.,0.,1.));
#7374=DIRECTION('center_axis',(-1.,0.,0.));
#7375=DIRECTION('ref_axis',(0.,-1.,0.));
#7376=DIRECTION('',(0.,-1.,0.));
#7377=DIRECTION('',(0.,-1.,0.));
#7378=DIRECTION('center_axis',(0.,0.,1.));
#7379=DIRECTION('ref_axis',(1.,0.,0.));
#7380=DIRECTION('center_axis',(0.,0.,1.));
#7381=DIRECTION('ref_axis',(1.,0.,0.));
#7382=DIRECTION('axis',(0.,0.,1.));
#7383=DIRECTION('refdir',(1.,0.,0.));
#7384=DIRECTION('center_axis',(0.,0.,1.));
#7385=DIRECTION('ref_axis',(1.,0.,0.));
#7386=DIRECTION('center_axis',(0.,0.,1.));
#7387=DIRECTION('ref_axis',(1.,0.,0.));
#7388=DIRECTION('',(0.,0.,1.));
#7389=DIRECTION('center_axis',(0.,0.,-1.));
#7390=DIRECTION('ref_axis',(1.,0.,0.));
#7391=DIRECTION('center_axis',(0.,0.,1.));
#7392=DIRECTION('ref_axis',(1.,0.,0.));
#7393=DIRECTION('center_axis',(0.,0.,1.));
#7394=DIRECTION('ref_axis',(1.,0.,0.));
#7395=DIRECTION('center_axis',(0.,0.,1.));
#7396=DIRECTION('ref_axis',(1.,0.,0.));
#7397=DIRECTION('',(0.,0.,1.));
#7398=DIRECTION('center_axis',(0.,0.,-1.));
#7399=DIRECTION('ref_axis',(1.,0.,0.));
#7400=DIRECTION('center_axis',(0.,0.,1.));
#7401=DIRECTION('ref_axis',(1.,0.,0.));
#7402=DIRECTION('center_axis',(0.,0.,1.));
#7403=DIRECTION('ref_axis',(1.,0.,0.));
#7404=DIRECTION('center_axis',(0.,0.,1.));
#7405=DIRECTION('ref_axis',(1.,0.,0.));
#7406=DIRECTION('center_axis',(0.,0.,1.));
#7407=DIRECTION('ref_axis',(1.,0.,0.));
#7408=DIRECTION('',(0.,0.,1.));
#7409=DIRECTION('center_axis',(0.,0.,-1.));
#7410=DIRECTION('ref_axis',(1.,0.,0.));
#7411=DIRECTION('center_axis',(0.,0.,1.));
#7412=DIRECTION('ref_axis',(1.,0.,0.));
#7413=DIRECTION('center_axis',(0.,0.,1.));
#7414=DIRECTION('ref_axis',(1.,0.,0.));
#7415=DIRECTION('center_axis',(0.,0.,1.));
#7416=DIRECTION('ref_axis',(1.,0.,0.));
#7417=DIRECTION('center_axis',(0.,0.,1.));
#7418=DIRECTION('ref_axis',(1.,0.,0.));
#7419=DIRECTION('',(0.,0.,1.));
#7420=DIRECTION('center_axis',(0.,0.,1.));
#7421=DIRECTION('ref_axis',(1.,0.,0.));
#7422=DIRECTION('center_axis',(0.,0.,1.));
#7423=DIRECTION('ref_axis',(1.,0.,0.));
#7424=DIRECTION('',(0.,0.,1.));
#7425=DIRECTION('center_axis',(0.,1.,0.));
#7426=DIRECTION('ref_axis',(-1.,0.,0.));
#7427=DIRECTION('',(-1.,0.,0.));
#7428=DIRECTION('',(0.,0.,1.));
#7429=DIRECTION('',(-1.,0.,0.));
#7430=DIRECTION('',(0.,0.,1.));
#7431=DIRECTION('center_axis',(1.,0.,0.));
#7432=DIRECTION('ref_axis',(0.,1.,0.));
#7433=DIRECTION('',(0.,1.,0.));
#7434=DIRECTION('',(0.,1.,0.));
#7435=DIRECTION('',(0.,0.,1.));
#7436=DIRECTION('center_axis',(0.,-1.,0.));
#7437=DIRECTION('ref_axis',(1.,0.,0.));
#7438=DIRECTION('',(1.,0.,0.));
#7439=DIRECTION('',(1.,0.,0.));
#7440=DIRECTION('',(0.,0.,1.));
#7441=DIRECTION('center_axis',(-1.,0.,0.));
#7442=DIRECTION('ref_axis',(0.,-1.,0.));
#7443=DIRECTION('',(0.,-1.,0.));
#7444=DIRECTION('',(0.,-1.,0.));
#7445=DIRECTION('center_axis',(0.,0.,1.));
#7446=DIRECTION('ref_axis',(1.,0.,0.));
#7447=DIRECTION('center_axis',(0.,0.,1.));
#7448=DIRECTION('ref_axis',(1.,0.,0.));
#7449=DIRECTION('axis',(0.,0.,1.));
#7450=DIRECTION('refdir',(1.,0.,0.));
#7451=DIRECTION('center_axis',(0.,1.,0.));
#7452=DIRECTION('ref_axis',(1.,0.,0.));
#7453=DIRECTION('',(-1.,0.,0.));
#7454=DIRECTION('center_axis',(0.,1.,0.));
#7455=DIRECTION('ref_axis',(1.,0.,0.));
#7456=DIRECTION('center_axis',(0.,1.,0.));
#7457=DIRECTION('ref_axis',(1.,0.,0.));
#7458=DIRECTION('',(0.,0.,-1.));
#7459=DIRECTION('center_axis',(0.,1.,0.));
#7460=DIRECTION('ref_axis',(1.,0.,0.));
#7461=DIRECTION('center_axis',(0.,1.,0.));
#7462=DIRECTION('ref_axis',(1.,0.,0.));
#7463=DIRECTION('',(-1.,0.,0.));
#7464=DIRECTION('center_axis',(0.,1.,0.));
#7465=DIRECTION('ref_axis',(1.,0.,0.));
#7466=DIRECTION('center_axis',(0.,1.,0.));
#7467=DIRECTION('ref_axis',(1.,0.,0.));
#7468=DIRECTION('',(0.,1.,0.));
#7469=DIRECTION('',(0.,-1.,0.));
#7470=DIRECTION('center_axis',(0.,0.707106781186548,0.707106781186547));
#7471=DIRECTION('ref_axis',(0.,0.707106781186547,-0.707106781186548));
#7472=DIRECTION('center_axis',(0.,0.707106781186548,-0.707106781186547));
#7473=DIRECTION('ref_axis',(0.,-0.707106781186547,-0.707106781186548));
#7474=DIRECTION('',(0.,1.,0.));
#7475=DIRECTION('center_axis',(0.,1.,0.));
#7476=DIRECTION('ref_axis',(1.,0.,0.));
#7477=DIRECTION('center_axis',(0.,0.707106781186548,0.707106781186547));
#7478=DIRECTION('ref_axis',(0.,0.707106781186547,-0.707106781186548));
#7479=DIRECTION('center_axis',(0.,1.,0.));
#7480=DIRECTION('ref_axis',(1.,0.,0.));
#7481=DIRECTION('center_axis',(0.,-0.707106781186548,-0.707106781186547));
#7482=DIRECTION('ref_axis',(0.,0.707106781186547,-0.707106781186548));
#7483=DIRECTION('center_axis',(0.,-0.707106781186548,0.707106781186547));
#7484=DIRECTION('ref_axis',(0.,-0.707106781186547,-0.707106781186548));
#7485=DIRECTION('center_axis',(0.,1.,0.));
#7486=DIRECTION('ref_axis',(-1.,0.,1.22464679914735E-16));
#7487=DIRECTION('center_axis',(0.,-0.707106781186548,-0.707106781186547));
#7488=DIRECTION('ref_axis',(0.,0.707106781186547,-0.707106781186548));
#7489=DIRECTION('center_axis',(0.,1.,0.));
#7490=DIRECTION('ref_axis',(1.,0.,0.));
#7491=DIRECTION('center_axis',(0.,-0.707106781186548,0.707106781186547));
#7492=DIRECTION('ref_axis',(0.,-0.707106781186547,-0.707106781186548));
#7493=DIRECTION('center_axis',(0.,1.,0.));
#7494=DIRECTION('ref_axis',(1.,0.,0.));
#7495=DIRECTION('',(1.,0.,0.));
#7496=DIRECTION('center_axis',(0.,1.,0.));
#7497=DIRECTION('ref_axis',(1.,0.,0.));
#7498=DIRECTION('',(0.,0.,1.));
#7499=DIRECTION('center_axis',(0.,0.,1.));
#7500=DIRECTION('ref_axis',(1.,0.,0.));
#7501=DIRECTION('center_axis',(0.,0.,1.));
#7502=DIRECTION('ref_axis',(1.,0.,0.));
#7503=DIRECTION('center_axis',(0.,0.,1.));
#7504=DIRECTION('ref_axis',(1.,0.,0.));
#7505=DIRECTION('center_axis',(0.,0.,1.));
#7506=DIRECTION('ref_axis',(1.,0.,0.));
#7507=DIRECTION('center_axis',(0.,0.,1.));
#7508=DIRECTION('ref_axis',(1.,0.,0.));
#7509=DIRECTION('center_axis',(0.,0.,1.));
#7510=DIRECTION('ref_axis',(1.,0.,0.));
#7511=DIRECTION('',(0.,0.,1.));
#7512=DIRECTION('center_axis',(0.,0.,-1.));
#7513=DIRECTION('ref_axis',(1.,0.,0.));
#7514=DIRECTION('center_axis',(0.,0.,1.));
#7515=DIRECTION('ref_axis',(-1.,1.22464679914735E-16,0.));
#7516=DIRECTION('center_axis',(0.,0.,1.));
#7517=DIRECTION('ref_axis',(1.,0.,0.));
#7518=DIRECTION('center_axis',(0.,0.,1.));
#7519=DIRECTION('ref_axis',(1.,0.,0.));
#7520=DIRECTION('center_axis',(0.,0.,1.));
#7521=DIRECTION('ref_axis',(1.,0.,0.));
#7522=DIRECTION('center_axis',(0.,0.,1.));
#7523=DIRECTION('ref_axis',(1.,0.,0.));
#7524=DIRECTION('',(0.,0.,1.));
#7525=DIRECTION('center_axis',(0.,0.,-1.));
#7526=DIRECTION('ref_axis',(1.,0.,0.));
#7527=DIRECTION('center_axis',(0.,0.,1.));
#7528=DIRECTION('ref_axis',(1.,0.,0.));
#7529=DIRECTION('center_axis',(0.,0.,1.));
#7530=DIRECTION('ref_axis',(1.,0.,0.));
#7531=DIRECTION('',(0.,0.,1.));
#7532=DIRECTION('center_axis',(0.,0.,-1.));
#7533=DIRECTION('ref_axis',(1.,0.,0.));
#7534=DIRECTION('center_axis',(0.,0.,1.));
#7535=DIRECTION('ref_axis',(1.,0.,0.));
#7536=DIRECTION('center_axis',(0.,0.,1.));
#7537=DIRECTION('ref_axis',(1.,0.,0.));
#7538=DIRECTION('',(0.,0.,1.));
#7539=DIRECTION('center_axis',(0.,0.,-1.));
#7540=DIRECTION('ref_axis',(1.,0.,0.));
#7541=DIRECTION('center_axis',(0.,0.,1.));
#7542=DIRECTION('ref_axis',(1.,0.,0.));
#7543=DIRECTION('center_axis',(0.,1.,0.));
#7544=DIRECTION('ref_axis',(1.,0.,0.));
#7545=DIRECTION('center_axis',(0.,1.,0.));
#7546=DIRECTION('ref_axis',(1.,0.,0.));
#7547=DIRECTION('',(0.,1.,0.));
#7548=DIRECTION('center_axis',(0.,1.,0.));
#7549=DIRECTION('ref_axis',(1.,0.,0.));
#7550=DIRECTION('center_axis',(0.,1.,0.));
#7551=DIRECTION('ref_axis',(1.,0.,0.));
#7552=DIRECTION('',(0.,1.,0.));
#7553=DIRECTION('center_axis',(0.,1.,0.));
#7554=DIRECTION('ref_axis',(1.,0.,0.));
#7555=DIRECTION('center_axis',(0.,1.,0.));
#7556=DIRECTION('ref_axis',(1.,0.,0.));
#7557=DIRECTION('center_axis',(0.,0.,1.));
#7558=DIRECTION('ref_axis',(1.,0.,0.));
#7559=DIRECTION('',(0.,0.,1.));
#7560=DIRECTION('center_axis',(0.,0.,-1.));
#7561=DIRECTION('ref_axis',(1.,0.,0.));
#7562=DIRECTION('center_axis',(0.,0.,1.));
#7563=DIRECTION('ref_axis',(1.,0.,0.));
#7564=DIRECTION('center_axis',(0.,0.,1.));
#7565=DIRECTION('ref_axis',(1.,0.,0.));
#7566=DIRECTION('',(0.,0.,1.));
#7567=DIRECTION('center_axis',(0.,0.,-1.));
#7568=DIRECTION('ref_axis',(1.,0.,0.));
#7569=DIRECTION('center_axis',(0.,0.,1.));
#7570=DIRECTION('ref_axis',(1.,0.,0.));
#7571=DIRECTION('center_axis',(0.,1.,0.));
#7572=DIRECTION('ref_axis',(1.,0.,0.));
#7573=DIRECTION('center_axis',(0.,1.,0.));
#7574=DIRECTION('ref_axis',(1.,0.,0.));
#7575=DIRECTION('',(0.,1.,0.));
#7576=DIRECTION('center_axis',(0.,1.,0.));
#7577=DIRECTION('ref_axis',(1.,0.,0.));
#7578=DIRECTION('center_axis',(0.,1.,0.));
#7579=DIRECTION('ref_axis',(1.,0.,0.));
#7580=DIRECTION('',(0.,1.,0.));
#7581=DIRECTION('center_axis',(0.,1.,0.));
#7582=DIRECTION('ref_axis',(1.,0.,0.));
#7583=DIRECTION('center_axis',(0.,1.,0.));
#7584=DIRECTION('ref_axis',(1.,0.,0.));
#7585=DIRECTION('center_axis',(0.,0.,1.));
#7586=DIRECTION('ref_axis',(1.,0.,0.));
#7587=DIRECTION('',(0.,0.,1.));
#7588=DIRECTION('center_axis',(0.,0.,-1.));
#7589=DIRECTION('ref_axis',(1.,0.,0.));
#7590=DIRECTION('center_axis',(0.,0.,1.));
#7591=DIRECTION('ref_axis',(1.,0.,0.));
#7592=DIRECTION('center_axis',(0.,0.,1.));
#7593=DIRECTION('ref_axis',(1.,0.,0.));
#7594=DIRECTION('',(0.,0.,1.));
#7595=DIRECTION('center_axis',(0.,0.,-1.));
#7596=DIRECTION('ref_axis',(1.,0.,0.));
#7597=DIRECTION('center_axis',(0.,0.,1.));
#7598=DIRECTION('ref_axis',(1.,0.,0.));
#7599=DIRECTION('center_axis',(0.,1.,0.));
#7600=DIRECTION('ref_axis',(1.,0.,0.));
#7601=DIRECTION('center_axis',(0.,1.,0.));
#7602=DIRECTION('ref_axis',(1.,0.,0.));
#7603=DIRECTION('',(0.,1.,0.));
#7604=DIRECTION('center_axis',(0.,1.,0.));
#7605=DIRECTION('ref_axis',(1.,0.,0.));
#7606=DIRECTION('center_axis',(0.,1.,0.));
#7607=DIRECTION('ref_axis',(1.,0.,0.));
#7608=DIRECTION('',(0.,1.,0.));
#7609=DIRECTION('center_axis',(0.,1.,0.));
#7610=DIRECTION('ref_axis',(1.,0.,0.));
#7611=DIRECTION('center_axis',(0.,1.,0.));
#7612=DIRECTION('ref_axis',(1.,0.,0.));
#7613=DIRECTION('center_axis',(0.,0.,1.));
#7614=DIRECTION('ref_axis',(1.,0.,0.));
#7615=DIRECTION('',(0.,0.,1.));
#7616=DIRECTION('center_axis',(0.,0.,-1.));
#7617=DIRECTION('ref_axis',(1.,0.,0.));
#7618=DIRECTION('center_axis',(0.,0.,1.));
#7619=DIRECTION('ref_axis',(1.,0.,0.));
#7620=DIRECTION('center_axis',(0.,0.,1.));
#7621=DIRECTION('ref_axis',(1.,0.,0.));
#7622=DIRECTION('',(0.,0.,1.));
#7623=DIRECTION('center_axis',(0.,0.,-1.));
#7624=DIRECTION('ref_axis',(1.,0.,0.));
#7625=DIRECTION('center_axis',(0.,0.,1.));
#7626=DIRECTION('ref_axis',(1.,0.,0.));
#7627=DIRECTION('center_axis',(0.,1.,0.));
#7628=DIRECTION('ref_axis',(1.,0.,0.));
#7629=DIRECTION('center_axis',(0.,1.,0.));
#7630=DIRECTION('ref_axis',(1.,0.,0.));
#7631=DIRECTION('',(0.,1.,0.));
#7632=DIRECTION('center_axis',(0.,1.,0.));
#7633=DIRECTION('ref_axis',(1.,0.,0.));
#7634=DIRECTION('center_axis',(0.,1.,0.));
#7635=DIRECTION('ref_axis',(1.,0.,0.));
#7636=DIRECTION('',(0.,1.,0.));
#7637=DIRECTION('center_axis',(0.,1.,0.));
#7638=DIRECTION('ref_axis',(1.,0.,0.));
#7639=DIRECTION('center_axis',(0.,1.,0.));
#7640=DIRECTION('ref_axis',(1.,0.,0.));
#7641=DIRECTION('center_axis',(1.,0.,0.));
#7642=DIRECTION('ref_axis',(0.,0.,-1.));
#7643=DIRECTION('center_axis',(1.,0.,0.));
#7644=DIRECTION('ref_axis',(0.,0.,-1.));
#7645=DIRECTION('',(1.,0.,0.));
#7646=DIRECTION('',(1.,0.,0.));
#7647=DIRECTION('',(1.,0.,0.));
#7648=DIRECTION('',(1.,0.,0.));
#7649=DIRECTION('',(1.,0.,0.));
#7650=DIRECTION('',(1.,0.,0.));
#7651=DIRECTION('center_axis',(-1.,0.,0.));
#7652=DIRECTION('ref_axis',(0.,0.,-1.));
#7653=DIRECTION('center_axis',(0.,0.,1.));
#7654=DIRECTION('ref_axis',(1.,0.,0.));
#7655=DIRECTION('center_axis',(0.,0.,1.));
#7656=DIRECTION('ref_axis',(1.,0.,0.));
#7657=DIRECTION('',(0.,0.,1.));
#7658=DIRECTION('center_axis',(0.,0.,-1.));
#7659=DIRECTION('ref_axis',(1.,0.,0.));
#7660=DIRECTION('center_axis',(0.,0.,1.));
#7661=DIRECTION('ref_axis',(1.,0.,0.));
#7662=DIRECTION('center_axis',(0.,0.,1.));
#7663=DIRECTION('ref_axis',(1.,0.,0.));
#7664=DIRECTION('center_axis',(0.,0.,1.));
#7665=DIRECTION('ref_axis',(1.,0.,0.));
#7666=DIRECTION('center_axis',(0.,0.,1.));
#7667=DIRECTION('ref_axis',(1.,0.,0.));
#7668=DIRECTION('',(0.,0.,1.));
#7669=DIRECTION('center_axis',(0.,0.,-1.));
#7670=DIRECTION('ref_axis',(1.,0.,0.));
#7671=DIRECTION('center_axis',(0.,0.,1.));
#7672=DIRECTION('ref_axis',(1.,0.,0.));
#7673=DIRECTION('center_axis',(0.,0.,1.));
#7674=DIRECTION('ref_axis',(1.,0.,0.));
#7675=DIRECTION('center_axis',(0.,0.,1.));
#7676=DIRECTION('ref_axis',(1.,0.,0.));
#7677=DIRECTION('center_axis',(0.,0.,1.));
#7678=DIRECTION('ref_axis',(1.,0.,0.));
#7679=DIRECTION('',(0.,0.,1.));
#7680=DIRECTION('center_axis',(0.,0.,-1.));
#7681=DIRECTION('ref_axis',(1.,0.,0.));
#7682=DIRECTION('center_axis',(0.,0.,1.));
#7683=DIRECTION('ref_axis',(1.,0.,0.));
#7684=DIRECTION('center_axis',(0.,0.,1.));
#7685=DIRECTION('ref_axis',(1.,0.,0.));
#7686=DIRECTION('center_axis',(0.,0.,1.));
#7687=DIRECTION('ref_axis',(1.,0.,0.));
#7688=DIRECTION('center_axis',(0.,0.,1.));
#7689=DIRECTION('ref_axis',(1.,0.,0.));
#7690=DIRECTION('',(0.,0.,1.));
#7691=DIRECTION('center_axis',(0.,0.,-1.));
#7692=DIRECTION('ref_axis',(1.,0.,0.));
#7693=DIRECTION('center_axis',(0.,0.,1.));
#7694=DIRECTION('ref_axis',(1.,0.,0.));
#7695=DIRECTION('center_axis',(0.,0.,1.));
#7696=DIRECTION('ref_axis',(1.,0.,0.));
#7697=DIRECTION('center_axis',(0.,0.,1.));
#7698=DIRECTION('ref_axis',(1.,0.,0.));
#7699=DIRECTION('center_axis',(0.,0.,1.));
#7700=DIRECTION('ref_axis',(1.,0.,0.));
#7701=DIRECTION('',(0.,0.,1.));
#7702=DIRECTION('center_axis',(0.,0.,1.));
#7703=DIRECTION('ref_axis',(1.,0.,0.));
#7704=DIRECTION('center_axis',(0.,0.,1.));
#7705=DIRECTION('ref_axis',(1.,0.,0.));
#7706=DIRECTION('',(0.,0.,1.));
#7707=DIRECTION('center_axis',(0.,0.,1.));
#7708=DIRECTION('ref_axis',(1.,0.,0.));
#7709=DIRECTION('center_axis',(0.,0.,1.));
#7710=DIRECTION('ref_axis',(1.,0.,0.));
#7711=DIRECTION('',(0.,0.,1.));
#7712=DIRECTION('center_axis',(0.,0.,1.));
#7713=DIRECTION('ref_axis',(1.,0.,0.));
#7714=DIRECTION('center_axis',(0.,0.,1.));
#7715=DIRECTION('ref_axis',(1.,0.,0.));
#7716=DIRECTION('',(0.,0.,1.));
#7717=DIRECTION('center_axis',(0.,1.,0.));
#7718=DIRECTION('ref_axis',(-1.,0.,0.));
#7719=DIRECTION('',(-1.,0.,0.));
#7720=DIRECTION('',(0.,0.,1.));
#7721=DIRECTION('',(-1.,0.,0.));
#7722=DIRECTION('',(0.,0.,1.));
#7723=DIRECTION('center_axis',(1.,0.,0.));
#7724=DIRECTION('ref_axis',(0.,1.,0.));
#7725=DIRECTION('',(0.,1.,0.));
#7726=DIRECTION('',(0.,1.,0.));
#7727=DIRECTION('',(0.,0.,1.));
#7728=DIRECTION('center_axis',(0.,-1.,0.));
#7729=DIRECTION('ref_axis',(1.,0.,0.));
#7730=DIRECTION('',(1.,0.,0.));
#7731=DIRECTION('',(1.,0.,0.));
#7732=DIRECTION('',(0.,0.,1.));
#7733=DIRECTION('center_axis',(-1.,0.,0.));
#7734=DIRECTION('ref_axis',(0.,-1.,0.));
#7735=DIRECTION('',(0.,-1.,0.));
#7736=DIRECTION('',(0.,-1.,0.));
#7737=DIRECTION('center_axis',(0.,0.,1.));
#7738=DIRECTION('ref_axis',(1.,0.,0.));
#7739=DIRECTION('center_axis',(0.,0.,1.));
#7740=DIRECTION('ref_axis',(1.,0.,0.));
#7741=DIRECTION('axis',(0.,0.,1.));
#7742=DIRECTION('refdir',(1.,0.,0.));
#7743=DIRECTION('center_axis',(0.,1.,0.));
#7744=DIRECTION('ref_axis',(1.,0.,0.));
#7745=DIRECTION('center_axis',(0.,-1.,0.));
#7746=DIRECTION('ref_axis',(1.,0.,0.));
#7747=DIRECTION('',(0.,-1.,0.));
#7748=DIRECTION('center_axis',(0.,-1.,0.));
#7749=DIRECTION('ref_axis',(1.,0.,0.));
#7750=DIRECTION('center_axis',(0.,1.,0.));
#7751=DIRECTION('ref_axis',(1.,0.,0.));
#7752=DIRECTION('center_axis',(0.,1.,0.));
#7753=DIRECTION('ref_axis',(1.,0.,0.));
#7754=DIRECTION('',(0.,-1.,0.));
#7755=DIRECTION('center_axis',(0.,1.,0.));
#7756=DIRECTION('ref_axis',(1.,0.,0.));
#7757=DIRECTION('center_axis',(0.,1.,0.));
#7758=DIRECTION('ref_axis',(1.,0.,0.));
#7759=DIRECTION('center_axis',(0.,1.,0.));
#7760=DIRECTION('ref_axis',(1.,0.,0.));
#7761=DIRECTION('axis',(0.,0.,1.));
#7762=DIRECTION('refdir',(1.,0.,0.));
#7763=DIRECTION('center_axis',(0.,0.,1.));
#7764=DIRECTION('ref_axis',(1.,0.,0.));
#7765=DIRECTION('center_axis',(0.,0.,1.));
#7766=DIRECTION('ref_axis',(1.,0.,0.));
#7767=DIRECTION('center_axis',(0.,0.,1.));
#7768=DIRECTION('ref_axis',(1.,0.,0.));
#7769=DIRECTION('center_axis',(0.,0.,1.));
#7770=DIRECTION('ref_axis',(1.,0.,0.));
#7771=DIRECTION('center_axis',(0.,0.,1.));
#7772=DIRECTION('ref_axis',(1.,0.,0.));
#7773=DIRECTION('',(0.,0.,-1.));
#7774=DIRECTION('center_axis',(0.,0.,1.));
#7775=DIRECTION('ref_axis',(1.,0.,0.));
#7776=DIRECTION('center_axis',(0.,0.,1.));
#7777=DIRECTION('ref_axis',(1.,0.,0.));
#7778=DIRECTION('center_axis',(0.,0.,1.));
#7779=DIRECTION('ref_axis',(1.,0.,0.));
#7780=DIRECTION('center_axis',(0.,0.,1.));
#7781=DIRECTION('ref_axis',(1.,0.,0.));
#7782=DIRECTION('center_axis',(0.,0.,1.));
#7783=DIRECTION('ref_axis',(1.,0.,0.));
#7784=DIRECTION('',(0.,0.,-1.));
#7785=DIRECTION('center_axis',(0.,0.,1.));
#7786=DIRECTION('ref_axis',(1.,0.,0.));
#7787=DIRECTION('',(0.,0.,-1.));
#7788=DIRECTION('center_axis',(0.,0.,1.));
#7789=DIRECTION('ref_axis',(1.,0.,0.));
#7790=DIRECTION('center_axis',(0.,0.,1.));
#7791=DIRECTION('ref_axis',(1.,0.,0.));
#7792=DIRECTION('axis',(0.,0.,1.));
#7793=DIRECTION('refdir',(1.,0.,0.));
#7794=DIRECTION('center_axis',(0.,0.,1.));
#7795=DIRECTION('ref_axis',(1.,0.,0.));
#7796=DIRECTION('center_axis',(0.,0.,-1.));
#7797=DIRECTION('ref_axis',(1.,0.,0.));
#7798=DIRECTION('',(0.,0.,-1.));
#7799=DIRECTION('center_axis',(0.,0.,-1.));
#7800=DIRECTION('ref_axis',(1.,0.,0.));
#7801=DIRECTION('center_axis',(0.,0.,1.));
#7802=DIRECTION('ref_axis',(1.,0.,0.));
#7803=DIRECTION('center_axis',(0.,0.,1.));
#7804=DIRECTION('ref_axis',(1.,0.,0.));
#7805=DIRECTION('',(0.,0.,-1.));
#7806=DIRECTION('center_axis',(0.,0.,1.));
#7807=DIRECTION('ref_axis',(1.,0.,0.));
#7808=DIRECTION('center_axis',(0.,0.,1.));
#7809=DIRECTION('ref_axis',(1.,0.,0.));
#7810=DIRECTION('center_axis',(0.,0.,1.));
#7811=DIRECTION('ref_axis',(1.,0.,0.));
#7812=DIRECTION('axis',(0.,0.,1.));
#7813=DIRECTION('refdir',(1.,0.,0.));
#7814=DIRECTION('center_axis',(0.,1.,0.));
#7815=DIRECTION('ref_axis',(1.,0.,0.));
#7816=DIRECTION('center_axis',(0.,-1.,0.));
#7817=DIRECTION('ref_axis',(1.,0.,0.));
#7818=DIRECTION('',(0.,-1.,0.));
#7819=DIRECTION('center_axis',(0.,-1.,0.));
#7820=DIRECTION('ref_axis',(1.,0.,0.));
#7821=DIRECTION('center_axis',(0.,1.,0.));
#7822=DIRECTION('ref_axis',(1.,0.,0.));
#7823=DIRECTION('center_axis',(0.,1.,0.));
#7824=DIRECTION('ref_axis',(1.,0.,0.));
#7825=DIRECTION('',(0.,-1.,0.));
#7826=DIRECTION('center_axis',(0.,1.,0.));
#7827=DIRECTION('ref_axis',(1.,0.,0.));
#7828=DIRECTION('center_axis',(0.,1.,0.));
#7829=DIRECTION('ref_axis',(1.,0.,0.));
#7830=DIRECTION('center_axis',(0.,1.,0.));
#7831=DIRECTION('ref_axis',(1.,0.,0.));
#7832=DIRECTION('axis',(0.,0.,1.));
#7833=DIRECTION('refdir',(1.,0.,0.));
#7834=DIRECTION('center_axis',(0.,0.,1.));
#7835=DIRECTION('ref_axis',(1.,0.,0.));
#7836=DIRECTION('center_axis',(0.,0.,1.));
#7837=DIRECTION('ref_axis',(1.,0.,0.));
#7838=DIRECTION('center_axis',(0.,0.,1.));
#7839=DIRECTION('ref_axis',(1.,0.,0.));
#7840=DIRECTION('center_axis',(0.,0.,1.));
#7841=DIRECTION('ref_axis',(1.,0.,0.));
#7842=DIRECTION('center_axis',(0.,0.,1.));
#7843=DIRECTION('ref_axis',(1.,0.,0.));
#7844=DIRECTION('',(0.,0.,-1.));
#7845=DIRECTION('center_axis',(0.,0.,1.));
#7846=DIRECTION('ref_axis',(1.,0.,0.));
#7847=DIRECTION('center_axis',(0.,0.,1.));
#7848=DIRECTION('ref_axis',(1.,0.,0.));
#7849=DIRECTION('center_axis',(0.,0.,1.));
#7850=DIRECTION('ref_axis',(1.,0.,0.));
#7851=DIRECTION('center_axis',(0.,0.,1.));
#7852=DIRECTION('ref_axis',(1.,0.,0.));
#7853=DIRECTION('center_axis',(0.,0.,1.));
#7854=DIRECTION('ref_axis',(1.,0.,0.));
#7855=DIRECTION('',(0.,0.,-1.));
#7856=DIRECTION('center_axis',(0.,0.,1.));
#7857=DIRECTION('ref_axis',(1.,0.,0.));
#7858=DIRECTION('',(0.,0.,-1.));
#7859=DIRECTION('center_axis',(0.,0.,1.));
#7860=DIRECTION('ref_axis',(1.,0.,0.));
#7861=DIRECTION('center_axis',(0.,0.,1.));
#7862=DIRECTION('ref_axis',(1.,0.,0.));
#7863=DIRECTION('axis',(0.,0.,1.));
#7864=DIRECTION('refdir',(1.,0.,0.));
#7865=DIRECTION('center_axis',(0.,0.,1.));
#7866=DIRECTION('ref_axis',(1.,0.,0.));
#7867=DIRECTION('center_axis',(0.,0.,-1.));
#7868=DIRECTION('ref_axis',(1.,0.,0.));
#7869=DIRECTION('',(0.,0.,-1.));
#7870=DIRECTION('center_axis',(0.,0.,-1.));
#7871=DIRECTION('ref_axis',(1.,0.,0.));
#7872=DIRECTION('center_axis',(0.,0.,1.));
#7873=DIRECTION('ref_axis',(1.,0.,0.));
#7874=DIRECTION('center_axis',(0.,0.,1.));
#7875=DIRECTION('ref_axis',(1.,0.,0.));
#7876=DIRECTION('',(0.,0.,-1.));
#7877=DIRECTION('center_axis',(0.,0.,1.));
#7878=DIRECTION('ref_axis',(1.,0.,0.));
#7879=DIRECTION('center_axis',(0.,0.,1.));
#7880=DIRECTION('ref_axis',(1.,0.,0.));
#7881=DIRECTION('center_axis',(0.,0.,1.));
#7882=DIRECTION('ref_axis',(1.,0.,0.));
#7883=DIRECTION('axis',(0.,0.,1.));
#7884=DIRECTION('refdir',(1.,0.,0.));
#7885=DIRECTION('center_axis',(0.,1.,0.));
#7886=DIRECTION('ref_axis',(1.,0.,0.));
#7887=DIRECTION('center_axis',(0.,-1.,0.));
#7888=DIRECTION('ref_axis',(1.,0.,0.));
#7889=DIRECTION('',(0.,-1.,0.));
#7890=DIRECTION('center_axis',(0.,-1.,0.));
#7891=DIRECTION('ref_axis',(1.,0.,0.));
#7892=DIRECTION('center_axis',(0.,1.,0.));
#7893=DIRECTION('ref_axis',(1.,0.,0.));
#7894=DIRECTION('center_axis',(0.,1.,0.));
#7895=DIRECTION('ref_axis',(1.,0.,0.));
#7896=DIRECTION('',(0.,-1.,0.));
#7897=DIRECTION('center_axis',(0.,1.,0.));
#7898=DIRECTION('ref_axis',(1.,0.,0.));
#7899=DIRECTION('center_axis',(0.,1.,0.));
#7900=DIRECTION('ref_axis',(1.,0.,0.));
#7901=DIRECTION('center_axis',(0.,1.,0.));
#7902=DIRECTION('ref_axis',(1.,0.,0.));
#7903=DIRECTION('axis',(0.,0.,1.));
#7904=DIRECTION('refdir',(1.,0.,0.));
#7905=DIRECTION('center_axis',(0.,0.,1.));
#7906=DIRECTION('ref_axis',(1.,0.,0.));
#7907=DIRECTION('center_axis',(0.,0.,1.));
#7908=DIRECTION('ref_axis',(1.,0.,0.));
#7909=DIRECTION('center_axis',(0.,0.,1.));
#7910=DIRECTION('ref_axis',(1.,0.,0.));
#7911=DIRECTION('center_axis',(0.,0.,1.));
#7912=DIRECTION('ref_axis',(1.,0.,0.));
#7913=DIRECTION('center_axis',(0.,0.,1.));
#7914=DIRECTION('ref_axis',(1.,0.,0.));
#7915=DIRECTION('',(0.,0.,-1.));
#7916=DIRECTION('center_axis',(0.,0.,1.));
#7917=DIRECTION('ref_axis',(1.,0.,0.));
#7918=DIRECTION('center_axis',(0.,0.,1.));
#7919=DIRECTION('ref_axis',(1.,0.,0.));
#7920=DIRECTION('center_axis',(0.,0.,1.));
#7921=DIRECTION('ref_axis',(1.,0.,0.));
#7922=DIRECTION('center_axis',(0.,0.,1.));
#7923=DIRECTION('ref_axis',(1.,0.,0.));
#7924=DIRECTION('center_axis',(0.,0.,1.));
#7925=DIRECTION('ref_axis',(1.,0.,0.));
#7926=DIRECTION('',(0.,0.,-1.));
#7927=DIRECTION('center_axis',(0.,0.,1.));
#7928=DIRECTION('ref_axis',(1.,0.,0.));
#7929=DIRECTION('',(0.,0.,-1.));
#7930=DIRECTION('center_axis',(0.,0.,1.));
#7931=DIRECTION('ref_axis',(1.,0.,0.));
#7932=DIRECTION('center_axis',(0.,0.,1.));
#7933=DIRECTION('ref_axis',(1.,0.,0.));
#7934=DIRECTION('axis',(0.,0.,1.));
#7935=DIRECTION('refdir',(1.,0.,0.));
#7936=DIRECTION('center_axis',(0.,0.,1.));
#7937=DIRECTION('ref_axis',(1.,0.,0.));
#7938=DIRECTION('center_axis',(0.,0.,-1.));
#7939=DIRECTION('ref_axis',(1.,0.,0.));
#7940=DIRECTION('',(0.,0.,-1.));
#7941=DIRECTION('center_axis',(0.,0.,-1.));
#7942=DIRECTION('ref_axis',(1.,0.,0.));
#7943=DIRECTION('center_axis',(0.,0.,1.));
#7944=DIRECTION('ref_axis',(1.,0.,0.));
#7945=DIRECTION('center_axis',(0.,0.,1.));
#7946=DIRECTION('ref_axis',(1.,0.,0.));
#7947=DIRECTION('',(0.,0.,-1.));
#7948=DIRECTION('center_axis',(0.,0.,1.));
#7949=DIRECTION('ref_axis',(1.,0.,0.));
#7950=DIRECTION('center_axis',(0.,0.,1.));
#7951=DIRECTION('ref_axis',(1.,0.,0.));
#7952=DIRECTION('center_axis',(0.,0.,1.));
#7953=DIRECTION('ref_axis',(1.,0.,0.));
#7954=DIRECTION('axis',(0.,0.,1.));
#7955=DIRECTION('refdir',(1.,0.,0.));
#7956=DIRECTION('center_axis',(0.,1.,0.));
#7957=DIRECTION('ref_axis',(1.,0.,0.));
#7958=DIRECTION('center_axis',(0.,-1.,0.));
#7959=DIRECTION('ref_axis',(1.,0.,0.));
#7960=DIRECTION('',(0.,-1.,0.));
#7961=DIRECTION('center_axis',(0.,-1.,0.));
#7962=DIRECTION('ref_axis',(1.,0.,0.));
#7963=DIRECTION('center_axis',(0.,1.,0.));
#7964=DIRECTION('ref_axis',(1.,0.,0.));
#7965=DIRECTION('center_axis',(0.,1.,0.));
#7966=DIRECTION('ref_axis',(1.,0.,0.));
#7967=DIRECTION('',(0.,-1.,0.));
#7968=DIRECTION('center_axis',(0.,1.,0.));
#7969=DIRECTION('ref_axis',(1.,0.,0.));
#7970=DIRECTION('center_axis',(0.,1.,0.));
#7971=DIRECTION('ref_axis',(1.,0.,0.));
#7972=DIRECTION('center_axis',(0.,1.,0.));
#7973=DIRECTION('ref_axis',(1.,0.,0.));
#7974=DIRECTION('axis',(0.,0.,1.));
#7975=DIRECTION('refdir',(1.,0.,0.));
#7976=DIRECTION('center_axis',(0.,0.,1.));
#7977=DIRECTION('ref_axis',(1.,0.,0.));
#7978=DIRECTION('center_axis',(0.,0.,1.));
#7979=DIRECTION('ref_axis',(1.,0.,0.));
#7980=DIRECTION('center_axis',(0.,0.,1.));
#7981=DIRECTION('ref_axis',(1.,0.,0.));
#7982=DIRECTION('center_axis',(0.,0.,1.));
#7983=DIRECTION('ref_axis',(1.,0.,0.));
#7984=DIRECTION('center_axis',(0.,0.,1.));
#7985=DIRECTION('ref_axis',(1.,0.,0.));
#7986=DIRECTION('',(0.,0.,-1.));
#7987=DIRECTION('center_axis',(0.,0.,1.));
#7988=DIRECTION('ref_axis',(1.,0.,0.));
#7989=DIRECTION('center_axis',(0.,0.,1.));
#7990=DIRECTION('ref_axis',(1.,0.,0.));
#7991=DIRECTION('center_axis',(0.,0.,1.));
#7992=DIRECTION('ref_axis',(1.,0.,0.));
#7993=DIRECTION('center_axis',(0.,0.,1.));
#7994=DIRECTION('ref_axis',(1.,0.,0.));
#7995=DIRECTION('center_axis',(0.,0.,1.));
#7996=DIRECTION('ref_axis',(1.,0.,0.));
#7997=DIRECTION('',(0.,0.,-1.));
#7998=DIRECTION('center_axis',(0.,0.,1.));
#7999=DIRECTION('ref_axis',(1.,0.,0.));
#8000=DIRECTION('',(0.,0.,-1.));
#8001=DIRECTION('center_axis',(0.,0.,1.));
#8002=DIRECTION('ref_axis',(1.,0.,0.));
#8003=DIRECTION('center_axis',(0.,0.,1.));
#8004=DIRECTION('ref_axis',(1.,0.,0.));
#8005=DIRECTION('axis',(0.,0.,1.));
#8006=DIRECTION('refdir',(1.,0.,0.));
#8007=DIRECTION('center_axis',(0.,0.,1.));
#8008=DIRECTION('ref_axis',(1.,0.,0.));
#8009=DIRECTION('center_axis',(0.,0.,-1.));
#8010=DIRECTION('ref_axis',(1.,0.,0.));
#8011=DIRECTION('',(0.,0.,-1.));
#8012=DIRECTION('center_axis',(0.,0.,-1.));
#8013=DIRECTION('ref_axis',(1.,0.,0.));
#8014=DIRECTION('center_axis',(0.,0.,1.));
#8015=DIRECTION('ref_axis',(1.,0.,0.));
#8016=DIRECTION('center_axis',(0.,0.,1.));
#8017=DIRECTION('ref_axis',(1.,0.,0.));
#8018=DIRECTION('',(0.,0.,-1.));
#8019=DIRECTION('center_axis',(0.,0.,1.));
#8020=DIRECTION('ref_axis',(1.,0.,0.));
#8021=DIRECTION('center_axis',(0.,0.,1.));
#8022=DIRECTION('ref_axis',(1.,0.,0.));
#8023=DIRECTION('center_axis',(0.,0.,1.));
#8024=DIRECTION('ref_axis',(1.,0.,0.));
#8025=DIRECTION('axis',(0.,0.,1.));
#8026=DIRECTION('refdir',(1.,0.,0.));
#8027=DIRECTION('center_axis',(1.,0.,0.));
#8028=DIRECTION('ref_axis',(0.,0.,-1.));
#8029=DIRECTION('center_axis',(1.,0.,0.));
#8030=DIRECTION('ref_axis',(0.,0.,-1.));
#8031=DIRECTION('',(-1.,0.,0.));
#8032=DIRECTION('center_axis',(1.,0.,0.));
#8033=DIRECTION('ref_axis',(0.,0.,-1.));
#8034=DIRECTION('center_axis',(1.,0.,0.));
#8035=DIRECTION('ref_axis',(0.,0.,-1.));
#8036=DIRECTION('center_axis',(1.,0.,0.));
#8037=DIRECTION('ref_axis',(0.,0.,-1.));
#8038=DIRECTION('axis',(0.,0.,1.));
#8039=DIRECTION('refdir',(1.,0.,0.));
#8040=DIRECTION('center_axis',(1.,0.,0.));
#8041=DIRECTION('ref_axis',(0.,0.,-1.));
#8042=DIRECTION('center_axis',(1.,0.,0.));
#8043=DIRECTION('ref_axis',(0.,0.,-1.));
#8044=DIRECTION('',(-1.,0.,0.));
#8045=DIRECTION('center_axis',(1.,0.,0.));
#8046=DIRECTION('ref_axis',(0.,0.,-1.));
#8047=DIRECTION('center_axis',(1.,0.,0.));
#8048=DIRECTION('ref_axis',(0.,0.,-1.));
#8049=DIRECTION('center_axis',(1.,0.,0.));
#8050=DIRECTION('ref_axis',(0.,0.,-1.));
#8051=DIRECTION('axis',(0.,0.,1.));
#8052=DIRECTION('refdir',(1.,0.,0.));
#8053=DIRECTION('center_axis',(0.,0.,1.));
#8054=DIRECTION('ref_axis',(1.,0.,0.));
#8055=DIRECTION('center_axis',(0.,0.,1.));
#8056=DIRECTION('ref_axis',(1.,0.,0.));
#8057=DIRECTION('',(0.,0.,1.));
#8058=DIRECTION('center_axis',(0.,0.,-1.));
#8059=DIRECTION('ref_axis',(1.,0.,0.));
#8060=DIRECTION('center_axis',(0.,0.,1.));
#8061=DIRECTION('ref_axis',(1.,0.,0.));
#8062=DIRECTION('center_axis',(0.,0.,1.));
#8063=DIRECTION('ref_axis',(1.,0.,0.));
#8064=DIRECTION('center_axis',(0.,0.,1.));
#8065=DIRECTION('ref_axis',(1.,0.,0.));
#8066=DIRECTION('',(0.,0.,1.));
#8067=DIRECTION('center_axis',(0.,0.,-1.));
#8068=DIRECTION('ref_axis',(1.,0.,0.));
#8069=DIRECTION('center_axis',(0.,0.,1.));
#8070=DIRECTION('ref_axis',(1.,0.,0.));
#8071=DIRECTION('center_axis',(0.,0.,1.));
#8072=DIRECTION('ref_axis',(1.,0.,0.));
#8073=DIRECTION('center_axis',(0.,0.,1.));
#8074=DIRECTION('ref_axis',(1.,0.,0.));
#8075=DIRECTION('',(0.,0.,1.));
#8076=DIRECTION('center_axis',(0.,0.,-1.));
#8077=DIRECTION('ref_axis',(1.,0.,0.));
#8078=DIRECTION('center_axis',(0.,0.,1.));
#8079=DIRECTION('ref_axis',(1.,0.,0.));
#8080=DIRECTION('center_axis',(0.,0.,1.));
#8081=DIRECTION('ref_axis',(1.,0.,0.));
#8082=DIRECTION('center_axis',(0.,0.,1.));
#8083=DIRECTION('ref_axis',(1.,0.,0.));
#8084=DIRECTION('',(0.,0.,1.));
#8085=DIRECTION('center_axis',(0.,0.,-1.));
#8086=DIRECTION('ref_axis',(1.,0.,0.));
#8087=DIRECTION('center_axis',(0.,0.,1.));
#8088=DIRECTION('ref_axis',(1.,0.,0.));
#8089=DIRECTION('center_axis',(0.,1.,0.));
#8090=DIRECTION('ref_axis',(1.,0.,0.));
#8091=DIRECTION('center_axis',(0.,1.,0.));
#8092=DIRECTION('ref_axis',(1.,0.,0.));
#8093=DIRECTION('',(0.,1.,0.));
#8094=DIRECTION('center_axis',(0.,1.,0.));
#8095=DIRECTION('ref_axis',(1.,0.,0.));
#8096=DIRECTION('center_axis',(0.,1.,0.));
#8097=DIRECTION('ref_axis',(1.,0.,0.));
#8098=DIRECTION('',(0.,1.,0.));
#8099=DIRECTION('center_axis',(0.,1.,0.));
#8100=DIRECTION('ref_axis',(1.,0.,0.));
#8101=DIRECTION('center_axis',(0.,1.,0.));
#8102=DIRECTION('ref_axis',(1.,0.,0.));
#8103=DIRECTION('',(0.,1.,0.));
#8104=DIRECTION('center_axis',(0.,1.,0.));
#8105=DIRECTION('ref_axis',(1.,0.,0.));
#8106=DIRECTION('center_axis',(0.,1.,0.));
#8107=DIRECTION('ref_axis',(1.,0.,0.));
#8108=DIRECTION('',(0.,1.,0.));
#8109=DIRECTION('center_axis',(-1.,0.,0.));
#8110=DIRECTION('ref_axis',(0.,0.,1.));
#8111=DIRECTION('',(0.,0.,-1.));
#8112=DIRECTION('',(0.,1.,0.));
#8113=DIRECTION('',(0.,0.,1.));
#8114=DIRECTION('',(0.,1.,0.));
#8115=DIRECTION('center_axis',(0.,0.,1.));
#8116=DIRECTION('ref_axis',(1.,0.,0.));
#8117=DIRECTION('center_axis',(0.,0.,-1.));
#8118=DIRECTION('ref_axis',(1.,0.,0.));
#8119=DIRECTION('',(0.,1.,0.));
#8120=DIRECTION('',(1.,0.,0.));
#8121=DIRECTION('center_axis',(0.,0.,-1.));
#8122=DIRECTION('ref_axis',(-1.,0.,0.));
#8123=DIRECTION('center_axis',(0.,0.,1.));
#8124=DIRECTION('ref_axis',(1.,0.,0.));
#8125=DIRECTION('',(-1.,0.,0.));
#8126=DIRECTION('',(0.,1.,0.));
#8127=DIRECTION('center_axis',(0.,0.,-1.));
#8128=DIRECTION('ref_axis',(-1.,0.,0.));
#8129=DIRECTION('center_axis',(0.,0.,1.));
#8130=DIRECTION('ref_axis',(1.,0.,0.));
#8131=DIRECTION('',(-1.,0.,0.));
#8132=DIRECTION('center_axis',(1.,0.,0.));
#8133=DIRECTION('ref_axis',(0.,0.,-1.));
#8134=DIRECTION('',(0.,0.,1.));
#8135=DIRECTION('',(0.,0.,-1.));
#8136=DIRECTION('center_axis',(0.,0.,1.));
#8137=DIRECTION('ref_axis',(1.,0.,0.));
#8138=DIRECTION('center_axis',(0.,0.,-1.));
#8139=DIRECTION('ref_axis',(1.,0.,0.));
#8140=DIRECTION('',(1.,0.,0.));
#8141=DIRECTION('center_axis',(0.,1.,0.));
#8142=DIRECTION('ref_axis',(0.,0.,1.));
#8143=DIRECTION('',(0.,0.,-1.));
#8144=DIRECTION('',(-1.,0.,0.));
#8145=DIRECTION('',(0.,0.,-1.));
#8146=DIRECTION('',(1.,0.,0.));
#8147=DIRECTION('',(0.,0.,-1.));
#8148=DIRECTION('center_axis',(1.,0.,0.));
#8149=DIRECTION('ref_axis',(0.,0.,-1.));
#8150=DIRECTION('',(0.,0.,-1.));
#8151=DIRECTION('',(0.,1.,0.));
#8152=DIRECTION('',(0.,1.,0.));
#8153=DIRECTION('center_axis',(0.,0.,-1.));
#8154=DIRECTION('ref_axis',(-1.,0.,0.));
#8155=DIRECTION('center_axis',(0.,0.,-1.));
#8156=DIRECTION('ref_axis',(1.,0.,0.));
#8157=DIRECTION('',(-1.,0.,0.));
#8158=DIRECTION('',(0.,1.,0.));
#8159=DIRECTION('center_axis',(-1.,0.,0.));
#8160=DIRECTION('ref_axis',(0.,0.,1.));
#8161=DIRECTION('',(0.,0.,1.));
#8162=DIRECTION('',(0.,0.,1.));
#8163=DIRECTION('',(0.,1.,0.));
#8164=DIRECTION('center_axis',(0.,0.,1.));
#8165=DIRECTION('ref_axis',(1.,0.,0.));
#8166=DIRECTION('center_axis',(0.,0.,1.));
#8167=DIRECTION('ref_axis',(1.,0.,0.));
#8168=DIRECTION('',(1.,0.,0.));
#8169=DIRECTION('center_axis',(0.,1.,0.));
#8170=DIRECTION('ref_axis',(0.,0.,1.));
#8171=DIRECTION('',(0.,0.,-1.));
#8172=DIRECTION('',(0.,0.,-1.));
#8173=DIRECTION('center_axis',(0.,0.,1.));
#8174=DIRECTION('ref_axis',(1.,0.,0.));
#8175=DIRECTION('center_axis',(0.,0.,1.));
#8176=DIRECTION('ref_axis',(1.,0.,0.));
#8177=DIRECTION('',(0.,0.,1.));
#8178=DIRECTION('center_axis',(0.,0.,-1.));
#8179=DIRECTION('ref_axis',(1.,0.,0.));
#8180=DIRECTION('center_axis',(0.,0.,1.));
#8181=DIRECTION('ref_axis',(6.12323399573677E-17,1.,0.));
#8182=DIRECTION('center_axis',(0.,0.,1.));
#8183=DIRECTION('ref_axis',(1.,0.,0.));
#8184=DIRECTION('',(0.,0.,1.));
#8185=DIRECTION('',(0.,0.,1.));
#8186=DIRECTION('center_axis',(0.,0.,-1.));
#8187=DIRECTION('ref_axis',(1.,0.,0.));
#8188=DIRECTION('center_axis',(0.,0.,1.));
#8189=DIRECTION('ref_axis',(1.,0.,0.));
#8190=DIRECTION('center_axis',(0.,0.,1.));
#8191=DIRECTION('ref_axis',(1.,0.,0.));
#8192=DIRECTION('center_axis',(0.,0.,1.));
#8193=DIRECTION('ref_axis',(1.,0.,0.));
#8194=DIRECTION('',(0.,0.,-1.));
#8195=DIRECTION('center_axis',(0.,0.,1.));
#8196=DIRECTION('ref_axis',(1.,0.,0.));
#8197=DIRECTION('center_axis',(0.,0.,1.));
#8198=DIRECTION('ref_axis',(1.,0.,0.));
#8199=DIRECTION('center_axis',(0.,0.,1.));
#8200=DIRECTION('ref_axis',(1.,0.,0.));
#8201=DIRECTION('axis',(0.,0.,1.));
#8202=DIRECTION('refdir',(1.,0.,0.));
#8203=DIRECTION('center_axis',(0.,1.,0.));
#8204=DIRECTION('ref_axis',(1.,0.,0.));
#8205=DIRECTION('center_axis',(0.,1.,0.));
#8206=DIRECTION('ref_axis',(1.,0.,0.));
#8207=DIRECTION('',(0.,1.,0.));
#8208=DIRECTION('center_axis',(0.,-1.,0.));
#8209=DIRECTION('ref_axis',(1.,0.,0.));
#8210=DIRECTION('center_axis',(0.,1.,0.));
#8211=DIRECTION('ref_axis',(1.,0.,0.));
#8212=DIRECTION('center_axis',(0.,1.,0.));
#8213=DIRECTION('ref_axis',(1.,0.,0.));
#8214=DIRECTION('',(0.,1.,0.));
#8215=DIRECTION('center_axis',(0.,-1.,0.));
#8216=DIRECTION('ref_axis',(1.,0.,0.));
#8217=DIRECTION('center_axis',(0.,1.,0.));
#8218=DIRECTION('ref_axis',(1.,0.,0.));
#8219=DIRECTION('center_axis',(0.,1.,0.));
#8220=DIRECTION('ref_axis',(1.,0.,0.));
#8221=DIRECTION('',(0.,1.,0.));
#8222=DIRECTION('center_axis',(0.,-1.,0.));
#8223=DIRECTION('ref_axis',(1.,0.,0.));
#8224=DIRECTION('center_axis',(0.,1.,0.));
#8225=DIRECTION('ref_axis',(1.,0.,0.));
#8226=DIRECTION('center_axis',(0.,1.,0.));
#8227=DIRECTION('ref_axis',(1.,0.,0.));
#8228=DIRECTION('',(0.,1.,0.));
#8229=DIRECTION('center_axis',(0.,-1.,0.));
#8230=DIRECTION('ref_axis',(1.,0.,0.));
#8231=DIRECTION('center_axis',(1.,0.,0.));
#8232=DIRECTION('ref_axis',(0.,0.,-1.));
#8233=DIRECTION('',(0.,0.,1.));
#8234=DIRECTION('',(0.,1.,0.));
#8235=DIRECTION('',(0.,0.,-1.));
#8236=DIRECTION('',(0.,1.,0.));
#8237=DIRECTION('center_axis',(0.,0.,1.));
#8238=DIRECTION('ref_axis',(1.,0.,0.));
#8239=DIRECTION('',(-1.,0.,0.));
#8240=DIRECTION('',(1.,0.,0.));
#8241=DIRECTION('',(0.,1.,0.));
#8242=DIRECTION('center_axis',(-1.,0.,0.));
#8243=DIRECTION('ref_axis',(0.,0.,1.));
#8244=DIRECTION('',(0.,0.,-1.));
#8245=DIRECTION('',(0.,0.,1.));
#8246=DIRECTION('',(0.,1.,0.));
#8247=DIRECTION('center_axis',(0.,0.,-1.));
#8248=DIRECTION('ref_axis',(-1.,0.,0.));
#8249=DIRECTION('',(1.,0.,0.));
#8250=DIRECTION('',(-1.,0.,0.));
#8251=DIRECTION('center_axis',(0.,1.,0.));
#8252=DIRECTION('ref_axis',(-1.,0.,0.));
#8253=DIRECTION('',(-1.,0.,0.));
#8254=DIRECTION('',(0.,0.,1.));
#8255=DIRECTION('',(-1.,0.,0.));
#8256=DIRECTION('',(0.,0.,1.));
#8257=DIRECTION('center_axis',(1.,0.,0.));
#8258=DIRECTION('ref_axis',(0.,1.,0.));
#8259=DIRECTION('',(0.,1.,0.));
#8260=DIRECTION('',(0.,1.,0.));
#8261=DIRECTION('',(0.,0.,1.));
#8262=DIRECTION('center_axis',(0.,-1.,0.));
#8263=DIRECTION('ref_axis',(1.,0.,0.));
#8264=DIRECTION('',(1.,0.,0.));
#8265=DIRECTION('',(1.,0.,0.));
#8266=DIRECTION('',(0.,0.,1.));
#8267=DIRECTION('center_axis',(-1.,0.,0.));
#8268=DIRECTION('ref_axis',(0.,-1.,0.));
#8269=DIRECTION('',(0.,-1.,0.));
#8270=DIRECTION('',(0.,-1.,0.));
#8271=DIRECTION('center_axis',(0.,0.,1.));
#8272=DIRECTION('ref_axis',(1.,0.,0.));
#8273=DIRECTION('center_axis',(0.,0.,1.));
#8274=DIRECTION('ref_axis',(1.,0.,0.));
#8275=DIRECTION('axis',(0.,0.,1.));
#8276=DIRECTION('refdir',(1.,0.,0.));
#8277=DIRECTION('center_axis',(0.,1.,0.));
#8278=DIRECTION('ref_axis',(1.,0.,0.));
#8279=DIRECTION('center_axis',(0.,1.,0.));
#8280=DIRECTION('ref_axis',(1.,0.,0.));
#8281=DIRECTION('',(0.,1.,0.));
#8282=DIRECTION('center_axis',(0.,-1.,0.));
#8283=DIRECTION('ref_axis',(1.,0.,0.));
#8284=DIRECTION('center_axis',(0.,1.,0.));
#8285=DIRECTION('ref_axis',(1.,0.,0.));
#8286=DIRECTION('center_axis',(0.,1.,0.));
#8287=DIRECTION('ref_axis',(1.,0.,0.));
#8288=DIRECTION('',(0.,1.,0.));
#8289=DIRECTION('center_axis',(0.,-1.,0.));
#8290=DIRECTION('ref_axis',(1.,0.,0.));
#8291=DIRECTION('center_axis',(0.,1.,0.));
#8292=DIRECTION('ref_axis',(1.,0.,0.));
#8293=DIRECTION('center_axis',(0.,1.,0.));
#8294=DIRECTION('ref_axis',(1.,0.,0.));
#8295=DIRECTION('',(0.,1.,0.));
#8296=DIRECTION('center_axis',(0.,-1.,0.));
#8297=DIRECTION('ref_axis',(1.,0.,0.));
#8298=DIRECTION('center_axis',(0.,1.,0.));
#8299=DIRECTION('ref_axis',(1.,0.,0.));
#8300=DIRECTION('center_axis',(0.,1.,0.));
#8301=DIRECTION('ref_axis',(1.,0.,0.));
#8302=DIRECTION('',(0.,1.,0.));
#8303=DIRECTION('center_axis',(0.,-1.,0.));
#8304=DIRECTION('ref_axis',(1.,0.,0.));
#8305=DIRECTION('center_axis',(0.,1.,0.));
#8306=DIRECTION('ref_axis',(-1.,0.,0.));
#8307=DIRECTION('',(-1.,0.,0.));
#8308=DIRECTION('',(0.,0.,1.));
#8309=DIRECTION('',(-1.,0.,0.));
#8310=DIRECTION('',(0.,0.,1.));
#8311=DIRECTION('center_axis',(1.,0.,0.));
#8312=DIRECTION('ref_axis',(0.,1.,0.));
#8313=DIRECTION('',(0.,1.,0.));
#8314=DIRECTION('',(0.,1.,0.));
#8315=DIRECTION('',(0.,0.,1.));
#8316=DIRECTION('center_axis',(0.,-1.,0.));
#8317=DIRECTION('ref_axis',(1.,0.,0.));
#8318=DIRECTION('',(1.,0.,0.));
#8319=DIRECTION('',(1.,0.,0.));
#8320=DIRECTION('',(0.,0.,1.));
#8321=DIRECTION('center_axis',(-1.,0.,0.));
#8322=DIRECTION('ref_axis',(0.,-1.,0.));
#8323=DIRECTION('',(0.,-1.,0.));
#8324=DIRECTION('',(0.,-1.,0.));
#8325=DIRECTION('center_axis',(0.,0.,1.));
#8326=DIRECTION('ref_axis',(1.,0.,0.));
#8327=DIRECTION('center_axis',(0.,0.,1.));
#8328=DIRECTION('ref_axis',(1.,0.,0.));
#8329=DIRECTION('axis',(0.,0.,1.));
#8330=DIRECTION('refdir',(1.,0.,0.));
#8331=DIRECTION('center_axis',(0.,1.,0.));
#8332=DIRECTION('ref_axis',(1.,0.,0.));
#8333=DIRECTION('center_axis',(0.,1.,0.));
#8334=DIRECTION('ref_axis',(1.,0.,0.));
#8335=DIRECTION('',(0.,1.,0.));
#8336=DIRECTION('center_axis',(0.,-1.,0.));
#8337=DIRECTION('ref_axis',(1.,0.,0.));
#8338=DIRECTION('center_axis',(0.,1.,0.));
#8339=DIRECTION('ref_axis',(1.,0.,0.));
#8340=DIRECTION('center_axis',(0.,1.,0.));
#8341=DIRECTION('ref_axis',(1.,0.,0.));
#8342=DIRECTION('',(0.,1.,0.));
#8343=DIRECTION('center_axis',(0.,-1.,0.));
#8344=DIRECTION('ref_axis',(1.,0.,0.));
#8345=DIRECTION('center_axis',(0.,1.,0.));
#8346=DIRECTION('ref_axis',(1.,0.,0.));
#8347=DIRECTION('center_axis',(0.,1.,0.));
#8348=DIRECTION('ref_axis',(1.,0.,0.));
#8349=DIRECTION('',(0.,1.,0.));
#8350=DIRECTION('center_axis',(0.,-1.,0.));
#8351=DIRECTION('ref_axis',(1.,0.,0.));
#8352=DIRECTION('center_axis',(0.,1.,0.));
#8353=DIRECTION('ref_axis',(1.,0.,0.));
#8354=DIRECTION('center_axis',(0.,1.,0.));
#8355=DIRECTION('ref_axis',(1.,0.,0.));
#8356=DIRECTION('',(0.,1.,0.));
#8357=DIRECTION('center_axis',(0.,-1.,0.));
#8358=DIRECTION('ref_axis',(1.,0.,0.));
#8359=DIRECTION('center_axis',(1.,0.,0.));
#8360=DIRECTION('ref_axis',(0.,0.,-1.));
#8361=DIRECTION('',(0.,0.,1.));
#8362=DIRECTION('',(0.,1.,0.));
#8363=DIRECTION('',(0.,0.,-1.));
#8364=DIRECTION('',(0.,1.,0.));
#8365=DIRECTION('center_axis',(0.,0.,1.));
#8366=DIRECTION('ref_axis',(1.,0.,0.));
#8367=DIRECTION('',(-1.,0.,0.));
#8368=DIRECTION('',(1.,0.,0.));
#8369=DIRECTION('',(0.,1.,0.));
#8370=DIRECTION('center_axis',(-1.,0.,0.));
#8371=DIRECTION('ref_axis',(0.,0.,1.));
#8372=DIRECTION('',(0.,0.,-1.));
#8373=DIRECTION('',(0.,0.,1.));
#8374=DIRECTION('',(0.,1.,0.));
#8375=DIRECTION('center_axis',(0.,0.,-1.));
#8376=DIRECTION('ref_axis',(-1.,0.,0.));
#8377=DIRECTION('',(1.,0.,0.));
#8378=DIRECTION('',(-1.,0.,0.));
#8379=DIRECTION('center_axis',(0.,1.,0.));
#8380=DIRECTION('ref_axis',(-1.,0.,0.));
#8381=DIRECTION('',(-1.,0.,0.));
#8382=DIRECTION('',(0.,0.,1.));
#8383=DIRECTION('',(-1.,0.,0.));
#8384=DIRECTION('',(0.,0.,1.));
#8385=DIRECTION('center_axis',(1.,0.,0.));
#8386=DIRECTION('ref_axis',(0.,1.,0.));
#8387=DIRECTION('',(0.,1.,0.));
#8388=DIRECTION('',(0.,1.,0.));
#8389=DIRECTION('',(0.,0.,1.));
#8390=DIRECTION('center_axis',(0.,-1.,0.));
#8391=DIRECTION('ref_axis',(1.,0.,0.));
#8392=DIRECTION('',(1.,0.,0.));
#8393=DIRECTION('',(1.,0.,0.));
#8394=DIRECTION('',(0.,0.,1.));
#8395=DIRECTION('center_axis',(-1.,0.,0.));
#8396=DIRECTION('ref_axis',(0.,-1.,0.));
#8397=DIRECTION('',(0.,-1.,0.));
#8398=DIRECTION('',(0.,-1.,0.));
#8399=DIRECTION('center_axis',(0.,0.,1.));
#8400=DIRECTION('ref_axis',(1.,0.,0.));
#8401=DIRECTION('center_axis',(0.,0.,1.));
#8402=DIRECTION('ref_axis',(1.,0.,0.));
#8403=DIRECTION('axis',(0.,0.,1.));
#8404=DIRECTION('refdir',(1.,0.,0.));
#8405=DIRECTION('center_axis',(-1.,0.,0.));
#8406=DIRECTION('ref_axis',(0.,0.,1.));
#8407=DIRECTION('',(0.,-1.,0.));
#8408=DIRECTION('',(0.,0.,1.));
#8409=DIRECTION('',(0.,1.,0.));
#8410=DIRECTION('',(0.,0.,1.));
#8411=DIRECTION('center_axis',(1.,0.,0.));
#8412=DIRECTION('ref_axis',(0.,0.,-1.));
#8413=DIRECTION('',(0.,1.,0.));
#8414=DIRECTION('',(0.,0.,-1.));
#8415=DIRECTION('',(0.,-1.,0.));
#8416=DIRECTION('',(0.,0.,-1.));
#8417=DIRECTION('center_axis',(0.,1.,0.));
#8418=DIRECTION('ref_axis',(0.,0.,1.));
#8419=DIRECTION('center_axis',(0.,1.,0.));
#8420=DIRECTION('ref_axis',(1.,0.,0.));
#8421=DIRECTION('center_axis',(0.,1.,0.));
#8422=DIRECTION('ref_axis',(1.,0.,0.));
#8423=DIRECTION('center_axis',(0.,1.,0.));
#8424=DIRECTION('ref_axis',(1.,0.,0.));
#8425=DIRECTION('center_axis',(0.,1.,0.));
#8426=DIRECTION('ref_axis',(1.,0.,0.));
#8427=DIRECTION('center_axis',(0.,1.,0.));
#8428=DIRECTION('ref_axis',(1.,0.,0.));
#8429=DIRECTION('center_axis',(0.,1.,0.));
#8430=DIRECTION('ref_axis',(1.,0.,0.));
#8431=DIRECTION('center_axis',(0.,1.,0.));
#8432=DIRECTION('ref_axis',(1.,0.,0.));
#8433=DIRECTION('center_axis',(0.,1.,0.));
#8434=DIRECTION('ref_axis',(1.,0.,0.));
#8435=DIRECTION('center_axis',(0.,1.,0.));
#8436=DIRECTION('ref_axis',(1.,0.,0.));
#8437=DIRECTION('center_axis',(0.,1.,0.));
#8438=DIRECTION('ref_axis',(1.,0.,0.));
#8439=DIRECTION('center_axis',(0.,1.,0.));
#8440=DIRECTION('ref_axis',(1.,0.,0.));
#8441=DIRECTION('',(0.,-1.,0.));
#8442=DIRECTION('center_axis',(0.,1.,0.));
#8443=DIRECTION('ref_axis',(1.,0.,0.));
#8444=DIRECTION('center_axis',(0.,1.,0.));
#8445=DIRECTION('ref_axis',(1.,0.,0.));
#8446=DIRECTION('',(0.,-1.,0.));
#8447=DIRECTION('center_axis',(0.,1.,0.));
#8448=DIRECTION('ref_axis',(1.,0.,0.));
#8449=DIRECTION('axis',(0.,0.,1.));
#8450=DIRECTION('refdir',(1.,0.,0.));
#8451=DIRECTION('center_axis',(-1.,0.,0.));
#8452=DIRECTION('ref_axis',(0.,0.,1.));
#8453=DIRECTION('',(0.,-1.,0.));
#8454=DIRECTION('',(0.,0.,1.));
#8455=DIRECTION('',(0.,1.,0.));
#8456=DIRECTION('',(0.,0.,1.));
#8457=DIRECTION('center_axis',(1.,0.,0.));
#8458=DIRECTION('ref_axis',(0.,0.,-1.));
#8459=DIRECTION('',(0.,1.,0.));
#8460=DIRECTION('',(0.,0.,-1.));
#8461=DIRECTION('',(0.,-1.,0.));
#8462=DIRECTION('',(0.,0.,-1.));
#8463=DIRECTION('center_axis',(0.,1.,0.));
#8464=DIRECTION('ref_axis',(0.,0.,1.));
#8465=DIRECTION('center_axis',(0.,1.,0.));
#8466=DIRECTION('ref_axis',(1.,0.,0.));
#8467=DIRECTION('center_axis',(0.,1.,0.));
#8468=DIRECTION('ref_axis',(1.,0.,0.));
#8469=DIRECTION('center_axis',(0.,1.,0.));
#8470=DIRECTION('ref_axis',(1.,0.,0.));
#8471=DIRECTION('center_axis',(0.,1.,0.));
#8472=DIRECTION('ref_axis',(1.,0.,0.));
#8473=DIRECTION('center_axis',(0.,1.,0.));
#8474=DIRECTION('ref_axis',(1.,0.,0.));
#8475=DIRECTION('center_axis',(0.,1.,0.));
#8476=DIRECTION('ref_axis',(1.,0.,0.));
#8477=DIRECTION('center_axis',(0.,1.,0.));
#8478=DIRECTION('ref_axis',(1.,0.,0.));
#8479=DIRECTION('center_axis',(0.,1.,0.));
#8480=DIRECTION('ref_axis',(1.,0.,0.));
#8481=DIRECTION('center_axis',(0.,1.,0.));
#8482=DIRECTION('ref_axis',(1.,0.,0.));
#8483=DIRECTION('center_axis',(0.,1.,0.));
#8484=DIRECTION('ref_axis',(1.,0.,0.));
#8485=DIRECTION('center_axis',(0.,1.,0.));
#8486=DIRECTION('ref_axis',(1.,0.,0.));
#8487=DIRECTION('',(0.,-1.,0.));
#8488=DIRECTION('center_axis',(0.,1.,0.));
#8489=DIRECTION('ref_axis',(1.,0.,0.));
#8490=DIRECTION('center_axis',(0.,1.,0.));
#8491=DIRECTION('ref_axis',(1.,0.,0.));
#8492=DIRECTION('',(0.,-1.,0.));
#8493=DIRECTION('center_axis',(0.,1.,0.));
#8494=DIRECTION('ref_axis',(1.,0.,0.));
#8495=DIRECTION('axis',(0.,0.,1.));
#8496=DIRECTION('refdir',(1.,0.,0.));
#8497=DIRECTION('center_axis',(-1.,0.,0.));
#8498=DIRECTION('ref_axis',(0.,0.,1.));
#8499=DIRECTION('',(0.,-1.,0.));
#8500=DIRECTION('',(0.,0.,1.));
#8501=DIRECTION('',(0.,1.,0.));
#8502=DIRECTION('',(0.,0.,1.));
#8503=DIRECTION('center_axis',(1.,0.,0.));
#8504=DIRECTION('ref_axis',(0.,0.,-1.));
#8505=DIRECTION('',(0.,1.,0.));
#8506=DIRECTION('',(0.,0.,-1.));
#8507=DIRECTION('',(0.,-1.,0.));
#8508=DIRECTION('',(0.,0.,-1.));
#8509=DIRECTION('center_axis',(0.,1.,0.));
#8510=DIRECTION('ref_axis',(0.,0.,1.));
#8511=DIRECTION('center_axis',(0.,1.,0.));
#8512=DIRECTION('ref_axis',(1.,0.,0.));
#8513=DIRECTION('center_axis',(0.,1.,0.));
#8514=DIRECTION('ref_axis',(1.,0.,0.));
#8515=DIRECTION('center_axis',(0.,1.,0.));
#8516=DIRECTION('ref_axis',(1.,0.,0.));
#8517=DIRECTION('center_axis',(0.,1.,0.));
#8518=DIRECTION('ref_axis',(1.,0.,0.));
#8519=DIRECTION('center_axis',(0.,1.,0.));
#8520=DIRECTION('ref_axis',(1.,0.,0.));
#8521=DIRECTION('center_axis',(0.,1.,0.));
#8522=DIRECTION('ref_axis',(1.,0.,0.));
#8523=DIRECTION('center_axis',(0.,1.,0.));
#8524=DIRECTION('ref_axis',(1.,0.,0.));
#8525=DIRECTION('center_axis',(0.,1.,0.));
#8526=DIRECTION('ref_axis',(1.,0.,0.));
#8527=DIRECTION('center_axis',(0.,1.,0.));
#8528=DIRECTION('ref_axis',(1.,0.,0.));
#8529=DIRECTION('center_axis',(0.,1.,0.));
#8530=DIRECTION('ref_axis',(1.,0.,0.));
#8531=DIRECTION('center_axis',(0.,1.,0.));
#8532=DIRECTION('ref_axis',(1.,0.,0.));
#8533=DIRECTION('',(0.,-1.,0.));
#8534=DIRECTION('center_axis',(0.,1.,0.));
#8535=DIRECTION('ref_axis',(1.,0.,0.));
#8536=DIRECTION('center_axis',(0.,1.,0.));
#8537=DIRECTION('ref_axis',(1.,0.,0.));
#8538=DIRECTION('',(0.,-1.,0.));
#8539=DIRECTION('center_axis',(0.,1.,0.));
#8540=DIRECTION('ref_axis',(1.,0.,0.));
#8541=DIRECTION('axis',(0.,0.,1.));
#8542=DIRECTION('refdir',(1.,0.,0.));
#8543=DIRECTION('center_axis',(-1.,0.,0.));
#8544=DIRECTION('ref_axis',(0.,0.,1.));
#8545=DIRECTION('',(0.,-1.,0.));
#8546=DIRECTION('',(0.,0.,1.));
#8547=DIRECTION('',(0.,1.,0.));
#8548=DIRECTION('',(0.,0.,1.));
#8549=DIRECTION('center_axis',(1.,0.,0.));
#8550=DIRECTION('ref_axis',(0.,0.,-1.));
#8551=DIRECTION('',(0.,1.,0.));
#8552=DIRECTION('',(0.,0.,-1.));
#8553=DIRECTION('',(0.,-1.,0.));
#8554=DIRECTION('',(0.,0.,-1.));
#8555=DIRECTION('center_axis',(0.,1.,0.));
#8556=DIRECTION('ref_axis',(0.,0.,1.));
#8557=DIRECTION('center_axis',(0.,1.,0.));
#8558=DIRECTION('ref_axis',(1.,0.,0.));
#8559=DIRECTION('center_axis',(0.,1.,0.));
#8560=DIRECTION('ref_axis',(1.,0.,0.));
#8561=DIRECTION('center_axis',(0.,1.,0.));
#8562=DIRECTION('ref_axis',(1.,0.,0.));
#8563=DIRECTION('center_axis',(0.,1.,0.));
#8564=DIRECTION('ref_axis',(1.,0.,0.));
#8565=DIRECTION('center_axis',(0.,1.,0.));
#8566=DIRECTION('ref_axis',(1.,0.,0.));
#8567=DIRECTION('center_axis',(0.,1.,0.));
#8568=DIRECTION('ref_axis',(1.,0.,0.));
#8569=DIRECTION('center_axis',(0.,1.,0.));
#8570=DIRECTION('ref_axis',(1.,0.,0.));
#8571=DIRECTION('center_axis',(0.,1.,0.));
#8572=DIRECTION('ref_axis',(1.,0.,0.));
#8573=DIRECTION('center_axis',(0.,1.,0.));
#8574=DIRECTION('ref_axis',(1.,0.,0.));
#8575=DIRECTION('center_axis',(0.,1.,0.));
#8576=DIRECTION('ref_axis',(1.,0.,0.));
#8577=DIRECTION('center_axis',(0.,1.,0.));
#8578=DIRECTION('ref_axis',(1.,0.,0.));
#8579=DIRECTION('',(0.,-1.,0.));
#8580=DIRECTION('center_axis',(0.,1.,0.));
#8581=DIRECTION('ref_axis',(1.,0.,0.));
#8582=DIRECTION('center_axis',(0.,1.,0.));
#8583=DIRECTION('ref_axis',(1.,0.,0.));
#8584=DIRECTION('',(0.,-1.,0.));
#8585=DIRECTION('center_axis',(0.,1.,0.));
#8586=DIRECTION('ref_axis',(1.,0.,0.));
#8587=DIRECTION('axis',(0.,0.,1.));
#8588=DIRECTION('refdir',(1.,0.,0.));
#8589=DIRECTION('center_axis',(0.,0.,1.));
#8590=DIRECTION('ref_axis',(1.,0.,0.));
#8591=DIRECTION('center_axis',(0.,0.,1.));
#8592=DIRECTION('ref_axis',(1.,0.,0.));
#8593=DIRECTION('',(0.,0.,1.));
#8594=DIRECTION('center_axis',(0.,0.,-1.));
#8595=DIRECTION('ref_axis',(1.,0.,0.));
#8596=DIRECTION('center_axis',(0.,0.,1.));
#8597=DIRECTION('ref_axis',(1.,0.,0.));
#8598=DIRECTION('center_axis',(0.,0.,1.));
#8599=DIRECTION('ref_axis',(1.,0.,0.));
#8600=DIRECTION('',(0.,0.,1.));
#8601=DIRECTION('center_axis',(0.,0.,-1.));
#8602=DIRECTION('ref_axis',(1.,0.,0.));
#8603=DIRECTION('center_axis',(0.,0.,1.));
#8604=DIRECTION('ref_axis',(1.,0.,0.));
#8605=DIRECTION('center_axis',(0.,0.,1.));
#8606=DIRECTION('ref_axis',(1.,0.,0.));
#8607=DIRECTION('',(0.,0.,1.));
#8608=DIRECTION('center_axis',(0.,0.,-1.));
#8609=DIRECTION('ref_axis',(1.,0.,0.));
#8610=DIRECTION('center_axis',(0.,0.,1.));
#8611=DIRECTION('ref_axis',(1.,0.,0.));
#8612=DIRECTION('center_axis',(0.,0.,1.));
#8613=DIRECTION('ref_axis',(1.,0.,0.));
#8614=DIRECTION('',(0.,0.,1.));
#8615=DIRECTION('center_axis',(0.,0.,-1.));
#8616=DIRECTION('ref_axis',(1.,0.,0.));
#8617=DIRECTION('center_axis',(0.,0.,1.));
#8618=DIRECTION('ref_axis',(1.,0.,0.));
#8619=DIRECTION('center_axis',(0.,0.,-1.));
#8620=DIRECTION('ref_axis',(1.,0.,0.));
#8621=DIRECTION('',(0.,0.,-1.));
#8622=DIRECTION('center_axis',(0.,0.,-1.));
#8623=DIRECTION('ref_axis',(1.,0.,0.));
#8624=DIRECTION('center_axis',(0.,0.,1.));
#8625=DIRECTION('ref_axis',(1.,0.,0.));
#8626=DIRECTION('center_axis',(0.,0.,1.));
#8627=DIRECTION('ref_axis',(1.,0.,0.));
#8628=DIRECTION('',(0.,0.,-1.));
#8629=DIRECTION('center_axis',(0.,0.,1.));
#8630=DIRECTION('ref_axis',(1.,0.,0.));
#8631=DIRECTION('center_axis',(0.,0.,1.));
#8632=DIRECTION('ref_axis',(1.,0.,0.));
#8633=DIRECTION('center_axis',(0.,0.,1.));
#8634=DIRECTION('ref_axis',(1.,0.,0.));
#8635=DIRECTION('axis',(0.,0.,1.));
#8636=DIRECTION('refdir',(1.,0.,0.));
#8637=DIRECTION('center_axis',(0.,0.,1.));
#8638=DIRECTION('ref_axis',(1.,0.,0.));
#8639=DIRECTION('center_axis',(0.,0.,1.));
#8640=DIRECTION('ref_axis',(1.,0.,0.));
#8641=DIRECTION('',(0.,0.,1.));
#8642=DIRECTION('center_axis',(0.,0.,-1.));
#8643=DIRECTION('ref_axis',(1.,0.,0.));
#8644=DIRECTION('center_axis',(0.,0.,1.));
#8645=DIRECTION('ref_axis',(1.,0.,0.));
#8646=DIRECTION('center_axis',(0.,0.,1.));
#8647=DIRECTION('ref_axis',(1.,0.,0.));
#8648=DIRECTION('',(0.,0.,1.));
#8649=DIRECTION('center_axis',(0.,0.,-1.));
#8650=DIRECTION('ref_axis',(1.,0.,0.));
#8651=DIRECTION('center_axis',(0.,0.,1.));
#8652=DIRECTION('ref_axis',(1.,0.,0.));
#8653=DIRECTION('center_axis',(0.,0.,1.));
#8654=DIRECTION('ref_axis',(1.,0.,0.));
#8655=DIRECTION('',(0.,0.,1.));
#8656=DIRECTION('center_axis',(0.,0.,-1.));
#8657=DIRECTION('ref_axis',(1.,0.,0.));
#8658=DIRECTION('center_axis',(0.,0.,1.));
#8659=DIRECTION('ref_axis',(1.,0.,0.));
#8660=DIRECTION('center_axis',(0.,0.,1.));
#8661=DIRECTION('ref_axis',(1.,0.,0.));
#8662=DIRECTION('',(0.,0.,1.));
#8663=DIRECTION('center_axis',(0.,0.,-1.));
#8664=DIRECTION('ref_axis',(1.,0.,0.));
#8665=DIRECTION('center_axis',(0.,0.,1.));
#8666=DIRECTION('ref_axis',(1.,0.,0.));
#8667=DIRECTION('center_axis',(0.,0.,1.));
#8668=DIRECTION('ref_axis',(1.,0.,0.));
#8669=DIRECTION('',(0.,0.,1.));
#8670=DIRECTION('center_axis',(0.,0.,-1.));
#8671=DIRECTION('ref_axis',(1.,0.,0.));
#8672=DIRECTION('center_axis',(0.,0.,1.));
#8673=DIRECTION('ref_axis',(1.,0.,0.));
#8674=DIRECTION('center_axis',(0.,0.,1.));
#8675=DIRECTION('ref_axis',(1.,0.,0.));
#8676=DIRECTION('',(0.,0.,-1.));
#8677=DIRECTION('center_axis',(0.,0.,1.));
#8678=DIRECTION('ref_axis',(1.,0.,0.));
#8679=DIRECTION('center_axis',(0.,0.,1.));
#8680=DIRECTION('ref_axis',(1.,0.,0.));
#8681=DIRECTION('center_axis',(0.,0.,1.));
#8682=DIRECTION('ref_axis',(1.,0.,0.));
#8683=DIRECTION('axis',(0.,0.,1.));
#8684=DIRECTION('refdir',(1.,0.,0.));
#8685=DIRECTION('center_axis',(0.,0.,1.));
#8686=DIRECTION('ref_axis',(1.,0.,0.));
#8687=DIRECTION('center_axis',(0.,0.,1.));
#8688=DIRECTION('ref_axis',(1.,0.,0.));
#8689=DIRECTION('',(0.,0.,1.));
#8690=DIRECTION('center_axis',(0.,0.,-1.));
#8691=DIRECTION('ref_axis',(1.,0.,0.));
#8692=DIRECTION('center_axis',(0.,0.,1.));
#8693=DIRECTION('ref_axis',(1.,0.,0.));
#8694=DIRECTION('center_axis',(0.,0.,1.));
#8695=DIRECTION('ref_axis',(1.,0.,0.));
#8696=DIRECTION('center_axis',(0.,0.,1.));
#8697=DIRECTION('ref_axis',(1.,0.,0.));
#8698=DIRECTION('center_axis',(0.,0.,1.));
#8699=DIRECTION('ref_axis',(1.,0.,0.));
#8700=DIRECTION('center_axis',(0.,0.,1.));
#8701=DIRECTION('ref_axis',(1.,0.,0.));
#8702=DIRECTION('',(0.,0.,-1.));
#8703=DIRECTION('center_axis',(0.,0.,1.));
#8704=DIRECTION('ref_axis',(1.,0.,0.));
#8705=DIRECTION('center_axis',(0.,0.,1.));
#8706=DIRECTION('ref_axis',(1.,0.,0.));
#8707=DIRECTION('',(0.,0.,-1.));
#8708=DIRECTION('center_axis',(0.,0.,1.));
#8709=DIRECTION('ref_axis',(1.,0.,0.));
#8710=DIRECTION('center_axis',(0.,0.,1.));
#8711=DIRECTION('ref_axis',(1.,0.,0.));
#8712=DIRECTION('axis',(0.,0.,1.));
#8713=DIRECTION('refdir',(1.,0.,0.));
#8714=DIRECTION('center_axis',(0.,1.,0.));
#8715=DIRECTION('ref_axis',(-1.,0.,0.));
#8716=DIRECTION('',(-1.,0.,0.));
#8717=DIRECTION('',(0.,0.,1.));
#8718=DIRECTION('',(-1.,0.,0.));
#8719=DIRECTION('',(0.,0.,1.));
#8720=DIRECTION('center_axis',(1.,0.,0.));
#8721=DIRECTION('ref_axis',(0.,1.,0.));
#8722=DIRECTION('',(0.,1.,0.));
#8723=DIRECTION('',(0.,1.,0.));
#8724=DIRECTION('',(0.,0.,1.));
#8725=DIRECTION('center_axis',(0.,-1.,0.));
#8726=DIRECTION('ref_axis',(1.,0.,0.));
#8727=DIRECTION('',(1.,0.,0.));
#8728=DIRECTION('',(1.,0.,0.));
#8729=DIRECTION('',(0.,0.,1.));
#8730=DIRECTION('center_axis',(-1.,0.,0.));
#8731=DIRECTION('ref_axis',(0.,-1.,0.));
#8732=DIRECTION('',(0.,-1.,0.));
#8733=DIRECTION('',(0.,-1.,0.));
#8734=DIRECTION('center_axis',(0.,0.,1.));
#8735=DIRECTION('ref_axis',(1.,0.,0.));
#8736=DIRECTION('center_axis',(0.,0.,1.));
#8737=DIRECTION('ref_axis',(1.,0.,0.));
#8738=DIRECTION('axis',(0.,0.,1.));
#8739=DIRECTION('refdir',(1.,0.,0.));
#8740=DIRECTION('center_axis',(0.,1.,0.));
#8741=DIRECTION('ref_axis',(-1.,0.,0.));
#8742=DIRECTION('',(-1.,0.,0.));
#8743=DIRECTION('',(0.,0.,1.));
#8744=DIRECTION('',(-1.,0.,0.));
#8745=DIRECTION('',(0.,0.,1.));
#8746=DIRECTION('center_axis',(1.,0.,0.));
#8747=DIRECTION('ref_axis',(0.,1.,0.));
#8748=DIRECTION('',(0.,1.,0.));
#8749=DIRECTION('',(0.,1.,0.));
#8750=DIRECTION('',(0.,0.,1.));
#8751=DIRECTION('center_axis',(0.,-1.,0.));
#8752=DIRECTION('ref_axis',(1.,0.,0.));
#8753=DIRECTION('',(1.,0.,0.));
#8754=DIRECTION('',(1.,0.,0.));
#8755=DIRECTION('',(0.,0.,1.));
#8756=DIRECTION('center_axis',(-1.,0.,0.));
#8757=DIRECTION('ref_axis',(0.,-1.,0.));
#8758=DIRECTION('',(0.,-1.,0.));
#8759=DIRECTION('',(0.,-1.,0.));
#8760=DIRECTION('center_axis',(0.,0.,1.));
#8761=DIRECTION('ref_axis',(1.,0.,0.));
#8762=DIRECTION('center_axis',(0.,0.,1.));
#8763=DIRECTION('ref_axis',(1.,0.,0.));
#8764=DIRECTION('axis',(0.,0.,1.));
#8765=DIRECTION('refdir',(1.,0.,0.));
#8766=DIRECTION('center_axis',(0.866025403784439,0.,-0.5));
#8767=DIRECTION('ref_axis',(0.5,0.,0.866025403784439));
#8768=DIRECTION('',(-0.5,0.,-0.866025403784439));
#8769=DIRECTION('',(0.,-1.,0.));
#8770=DIRECTION('',(0.5,0.,0.866025403784439));
#8771=DIRECTION('',(0.,-1.,0.));
#8772=DIRECTION('center_axis',(1.20185167898973E-16,0.,-1.));
#8773=DIRECTION('ref_axis',(1.,0.,1.20185167898973E-16));
#8774=DIRECTION('',(-1.,0.,-1.20185167898973E-16));
#8775=DIRECTION('',(0.,-1.,0.));
#8776=DIRECTION('',(1.,0.,1.20185167898973E-16));
#8777=DIRECTION('center_axis',(-0.866025403784439,0.,-0.5));
#8778=DIRECTION('ref_axis',(0.5,0.,-0.866025403784439));
#8779=DIRECTION('',(-0.5,0.,0.866025403784439));
#8780=DIRECTION('',(0.,-1.,0.));
#8781=DIRECTION('',(0.5,0.,-0.866025403784439));
#8782=DIRECTION('center_axis',(-0.866025403784439,0.,0.5));
#8783=DIRECTION('ref_axis',(-0.5,0.,-0.866025403784439));
#8784=DIRECTION('',(0.5,0.,0.866025403784439));
#8785=DIRECTION('',(0.,-1.,0.));
#8786=DIRECTION('',(-0.5,0.,-0.866025403784439));
#8787=DIRECTION('center_axis',(-2.40370335797945E-16,0.,1.));
#8788=DIRECTION('ref_axis',(-1.,0.,-2.40370335797945E-16));
#8789=DIRECTION('',(1.,0.,2.40370335797945E-16));
#8790=DIRECTION('',(0.,-1.,0.));
#8791=DIRECTION('',(-1.,0.,-2.40370335797945E-16));
#8792=DIRECTION('center_axis',(0.866025403784439,0.,0.5));
#8793=DIRECTION('ref_axis',(-0.5,0.,0.866025403784439));
#8794=DIRECTION('',(0.5,0.,-0.866025403784439));
#8795=DIRECTION('',(-0.5,0.,0.866025403784439));
#8796=DIRECTION('center_axis',(0.,1.,0.));
#8797=DIRECTION('ref_axis',(1.,0.,0.));
#8798=DIRECTION('center_axis',(0.,-1.,0.));
#8799=DIRECTION('ref_axis',(0.,0.,-1.));
#8800=DIRECTION('center_axis',(0.,1.,0.));
#8801=DIRECTION('ref_axis',(1.,0.,0.));
#8802=DIRECTION('center_axis',(0.,1.,0.));
#8803=DIRECTION('ref_axis',(1.,0.,0.));
#8804=DIRECTION('center_axis',(0.,1.,0.));
#8805=DIRECTION('ref_axis',(0.,0.,1.));
#8806=DIRECTION('center_axis',(0.,-1.,0.));
#8807=DIRECTION('ref_axis',(1.,0.,0.));
#8808=DIRECTION('center_axis',(0.,-1.,0.));
#8809=DIRECTION('ref_axis',(1.,0.,0.));
#8810=DIRECTION('center_axis',(0.,-1.,0.));
#8811=DIRECTION('ref_axis',(1.,0.,0.));
#8812=DIRECTION('',(0.707106781186548,0.707106781186547,8.65956056235493E-17));
#8813=DIRECTION('center_axis',(0.,-1.,0.));
#8814=DIRECTION('ref_axis',(1.,0.,0.));
#8815=DIRECTION('center_axis',(0.,-1.,0.));
#8816=DIRECTION('ref_axis',(1.,0.,0.));
#8817=DIRECTION('',(0.,1.,0.));
#8818=DIRECTION('center_axis',(0.,1.,0.));
#8819=DIRECTION('ref_axis',(1.,0.,0.));
#8820=DIRECTION('center_axis',(0.,-1.,0.));
#8821=DIRECTION('ref_axis',(1.,0.,0.));
#8822=DIRECTION('',(-0.707106781186547,0.707106781186548,-8.65956056235493E-17));
#8823=DIRECTION('center_axis',(0.,-1.,0.));
#8824=DIRECTION('ref_axis',(0.,0.,-1.));
#8825=DIRECTION('center_axis',(0.,-1.,0.));
#8826=DIRECTION('ref_axis',(1.,0.,0.));
#8827=DIRECTION('center_axis',(0.,1.,0.));
#8828=DIRECTION('ref_axis',(1.,0.,0.));
#8829=DIRECTION('center_axis',(0.,1.,0.));
#8830=DIRECTION('ref_axis',(1.,0.,0.));
#8831=DIRECTION('',(-0.447213595499958,0.894427190999916,-5.47678698264203E-17));
#8832=DIRECTION('center_axis',(0.,-1.,0.));
#8833=DIRECTION('ref_axis',(1.,0.,0.));
#8834=DIRECTION('',(0.,1.,0.));
#8835=DIRECTION('axis',(0.,0.,1.));
#8836=DIRECTION('refdir',(1.,0.,0.));
#8837=DIRECTION('axis',(0.,0.,1.));
#8838=DIRECTION('refdir',(1.,0.,0.));
#8839=DIRECTION('center_axis',(0.,1.,0.));
#8840=DIRECTION('ref_axis',(1.,0.,0.));
#8841=DIRECTION('center_axis',(0.,1.,0.));
#8842=DIRECTION('ref_axis',(1.,0.,0.));
#8843=DIRECTION('',(0.,1.,0.));
#8844=DIRECTION('center_axis',(0.,-1.,0.));
#8845=DIRECTION('ref_axis',(1.,0.,0.));
#8846=DIRECTION('center_axis',(0.,1.,0.));
#8847=DIRECTION('ref_axis',(1.,0.,0.));
#8848=DIRECTION('center_axis',(0.,1.,0.));
#8849=DIRECTION('ref_axis',(1.,0.,0.));
#8850=DIRECTION('center_axis',(0.,1.,0.));
#8851=DIRECTION('ref_axis',(1.,0.,0.));
#8852=DIRECTION('',(0.5,0.,-0.866025403784439));
#8853=DIRECTION('',(-0.5,0.,-0.866025403784439));
#8854=DIRECTION('',(-1.,0.,-1.60246890531964E-16));
#8855=DIRECTION('',(-0.5,0.,0.866025403784439));
#8856=DIRECTION('',(0.5,0.,0.866025403784439));
#8857=DIRECTION('',(1.,0.,1.60246890531964E-16));
#8858=DIRECTION('center_axis',(0.,-1.,0.));
#8859=DIRECTION('ref_axis',(1.,0.,0.));
#8860=DIRECTION('center_axis',(0.,1.,0.));
#8861=DIRECTION('ref_axis',(1.,0.,0.));
#8862=DIRECTION('',(0.5,0.,-0.866025403784439));
#8863=DIRECTION('',(1.,0.,1.60246890531964E-16));
#8864=DIRECTION('',(0.5,0.,0.866025403784439));
#8865=DIRECTION('',(-0.5,0.,0.866025403784439));
#8866=DIRECTION('',(-1.,0.,-1.60246890531964E-16));
#8867=DIRECTION('',(-0.5,0.,-0.866025403784439));
#8868=DIRECTION('center_axis',(0.,-1.,0.));
#8869=DIRECTION('ref_axis',(1.,0.,0.));
#8870=DIRECTION('center_axis',(-1.60246890531964E-16,0.,1.));
#8871=DIRECTION('ref_axis',(1.,0.,1.60246890531964E-16));
#8872=DIRECTION('',(0.,1.,0.));
#8873=DIRECTION('',(0.,1.,0.));
#8874=DIRECTION('center_axis',(-0.866025403784439,0.,0.5));
#8875=DIRECTION('ref_axis',(0.5,0.,0.866025403784439));
#8876=DIRECTION('',(0.,1.,0.));
#8877=DIRECTION('center_axis',(-0.866025403784439,0.,-0.5));
#8878=DIRECTION('ref_axis',(-0.5,0.,0.866025403784439));
#8879=DIRECTION('',(0.,1.,0.));
#8880=DIRECTION('center_axis',(1.60246890531964E-16,0.,-1.));
#8881=DIRECTION('ref_axis',(-1.,0.,-1.60246890531964E-16));
#8882=DIRECTION('',(0.,1.,0.));
#8883=DIRECTION('center_axis',(0.866025403784439,0.,-0.5));
#8884=DIRECTION('ref_axis',(-0.5,0.,-0.866025403784439));
#8885=DIRECTION('',(0.,1.,0.));
#8886=DIRECTION('center_axis',(0.866025403784439,0.,0.5));
#8887=DIRECTION('ref_axis',(0.5,0.,-0.866025403784439));
#8888=DIRECTION('center_axis',(0.,1.,0.));
#8889=DIRECTION('ref_axis',(0.,0.,1.));
#8890=DIRECTION('center_axis',(0.,-1.,0.));
#8891=DIRECTION('ref_axis',(1.,0.,0.));
#8892=DIRECTION('center_axis',(0.,-1.,0.));
#8893=DIRECTION('ref_axis',(1.,0.,0.));
#8894=DIRECTION('',(0.,1.,0.));
#8895=DIRECTION('center_axis',(0.,-1.,0.));
#8896=DIRECTION('ref_axis',(1.,0.,0.));
#8897=DIRECTION('center_axis',(0.,1.,0.));
#8898=DIRECTION('ref_axis',(0.,0.,1.));
#8899=DIRECTION('center_axis',(0.,-1.,0.));
#8900=DIRECTION('ref_axis',(1.,0.,0.));
#8901=DIRECTION('center_axis',(0.,-1.,0.));
#8902=DIRECTION('ref_axis',(1.,0.,0.));
#8903=DIRECTION('',(0.,1.,0.));
#8904=DIRECTION('center_axis',(0.,-1.,0.));
#8905=DIRECTION('ref_axis',(1.,0.,0.));
#8906=DIRECTION('center_axis',(0.,-1.,0.));
#8907=DIRECTION('ref_axis',(1.,0.,0.));
#8908=DIRECTION('',(0.,1.,0.));
#8909=DIRECTION('center_axis',(0.,-1.,0.));
#8910=DIRECTION('ref_axis',(0.,0.,-1.));
#8911=DIRECTION('center_axis',(0.,-1.,0.));
#8912=DIRECTION('ref_axis',(1.,0.,0.));
#8913=DIRECTION('center_axis',(0.,-1.,0.));
#8914=DIRECTION('ref_axis',(1.,0.,0.));
#8915=DIRECTION('',(0.,1.,0.));
#8916=DIRECTION('axis',(0.,0.,1.));
#8917=DIRECTION('refdir',(1.,0.,0.));
#8918=DIRECTION('center_axis',(0.,1.,0.));
#8919=DIRECTION('ref_axis',(0.,0.,1.));
#8920=DIRECTION('center_axis',(0.,-1.,0.));
#8921=DIRECTION('ref_axis',(1.,0.,0.));
#8922=DIRECTION('center_axis',(0.,-1.,0.));
#8923=DIRECTION('ref_axis',(1.,0.,0.));
#8924=DIRECTION('center_axis',(0.,-1.,0.));
#8925=DIRECTION('ref_axis',(1.,0.,0.));
#8926=DIRECTION('center_axis',(0.,-1.,0.));
#8927=DIRECTION('ref_axis',(1.,0.,0.));
#8928=DIRECTION('',(0.,1.,0.));
#8929=DIRECTION('center_axis',(0.,-1.,0.));
#8930=DIRECTION('ref_axis',(0.,0.,-1.));
#8931=DIRECTION('center_axis',(0.,-1.,0.));
#8932=DIRECTION('ref_axis',(1.,0.,0.));
#8933=DIRECTION('center_axis',(0.,-1.,0.));
#8934=DIRECTION('ref_axis',(1.,0.,0.));
#8935=DIRECTION('center_axis',(0.,-1.,0.));
#8936=DIRECTION('ref_axis',(1.,0.,0.));
#8937=DIRECTION('',(0.,1.,0.));
#8938=DIRECTION('center_axis',(0.,-1.,0.));
#8939=DIRECTION('ref_axis',(0.,0.,-1.));
#8940=DIRECTION('center_axis',(0.,-1.,0.));
#8941=DIRECTION('ref_axis',(1.,0.,0.));
#8942=DIRECTION('center_axis',(0.,-1.,0.));
#8943=DIRECTION('ref_axis',(1.,0.,0.));
#8944=DIRECTION('',(0.,1.,0.));
#8945=DIRECTION('',(0.,0.,1.));
#8946=DIRECTION('',(1.,0.,0.));
#8947=DIRECTION('',(0.,0.,1.));
#8948=DIRECTION('',(1.,0.,0.));
#8949=DIRECTION('axis',(0.,0.,1.));
#8950=DIRECTION('refdir',(1.,0.,0.));
#8951=DIRECTION('center_axis',(0.,1.,0.));
#8952=DIRECTION('ref_axis',(1.,0.,0.));
#8953=DIRECTION('',(-0.5,0.,0.866025403784439));
#8954=DIRECTION('',(-1.,0.,-3.29650746237182E-16));
#8955=DIRECTION('',(-0.5,0.,-0.866025403784439));
#8956=DIRECTION('',(0.5,0.,-0.866025403784438));
#8957=DIRECTION('',(1.,0.,0.));
#8958=DIRECTION('',(0.5,0.,0.866025403784439));
#8959=DIRECTION('center_axis',(0.,-1.,0.));
#8960=DIRECTION('ref_axis',(1.,0.,0.));
#8961=DIRECTION('center_axis',(0.,1.,0.));
#8962=DIRECTION('ref_axis',(1.,0.,0.));
#8963=DIRECTION('',(0.5,0.,-0.866025403784439));
#8964=DIRECTION('',(-0.5,0.,-0.866025403784439));
#8965=DIRECTION('',(-1.,0.,0.));
#8966=DIRECTION('',(-0.5,0.,0.866025403784438));
#8967=DIRECTION('',(0.5,0.,0.866025403784439));
#8968=DIRECTION('',(1.,0.,3.29650746237182E-16));
#8969=DIRECTION('center_axis',(0.,1.,0.));
#8970=DIRECTION('ref_axis',(1.,0.,0.));
#8971=DIRECTION('center_axis',(-3.29650746237182E-16,0.,1.));
#8972=DIRECTION('ref_axis',(1.,0.,3.29650746237182E-16));
#8973=DIRECTION('',(0.,-1.,0.));
#8974=DIRECTION('',(0.,1.,0.));
#8975=DIRECTION('center_axis',(-0.866025403784439,0.,0.5));
#8976=DIRECTION('ref_axis',(0.5,0.,0.866025403784439));
#8977=DIRECTION('',(0.,1.,0.));
#8978=DIRECTION('center_axis',(-0.866025403784439,0.,-0.5));
#8979=DIRECTION('ref_axis',(-0.5,0.,0.866025403784439));
#8980=DIRECTION('',(0.,1.,0.));
#8981=DIRECTION('center_axis',(0.,0.,-1.));
#8982=DIRECTION('ref_axis',(-1.,0.,0.));
#8983=DIRECTION('',(0.,1.,0.));
#8984=DIRECTION('center_axis',(0.866025403784439,0.,-0.5));
#8985=DIRECTION('ref_axis',(-0.5,0.,-0.866025403784439));
#8986=DIRECTION('',(0.,1.,0.));
#8987=DIRECTION('center_axis',(0.866025403784439,0.,0.5));
#8988=DIRECTION('ref_axis',(0.5,0.,-0.866025403784439));
#8989=DIRECTION('center_axis',(0.,-1.,0.));
#8990=DIRECTION('ref_axis',(1.,0.,0.));
#8991=DIRECTION('',(0.,1.,0.));
#8992=DIRECTION('center_axis',(0.,-1.,0.));
#8993=DIRECTION('ref_axis',(1.,0.,0.));
#8994=DIRECTION('center_axis',(0.,1.,0.));
#8995=DIRECTION('ref_axis',(0.,0.,1.));
#8996=DIRECTION('center_axis',(0.,-1.,0.));
#8997=DIRECTION('ref_axis',(1.,0.,0.));
#8998=DIRECTION('center_axis',(0.,-1.,0.));
#8999=DIRECTION('ref_axis',(1.,0.,0.));
#9000=DIRECTION('center_axis',(0.,-1.,0.));
#9001=DIRECTION('ref_axis',(1.,0.,0.));
#9002=DIRECTION('',(0.707106781186547,0.707106781186548,8.65956056235493E-17));
#9003=DIRECTION('center_axis',(0.,-1.,0.));
#9004=DIRECTION('ref_axis',(1.,0.,0.));
#9005=DIRECTION('center_axis',(0.,-1.,0.));
#9006=DIRECTION('ref_axis',(1.,0.,0.));
#9007=DIRECTION('',(0.,1.,0.));
#9008=DIRECTION('center_axis',(0.,1.,0.));
#9009=DIRECTION('ref_axis',(1.,0.,0.));
#9010=DIRECTION('center_axis',(0.,-1.,0.));
#9011=DIRECTION('ref_axis',(1.,0.,0.));
#9012=DIRECTION('',(-0.707106781186547,0.707106781186548,-8.65956056235493E-17));
#9013=DIRECTION('center_axis',(0.,-1.,0.));
#9014=DIRECTION('ref_axis',(0.,0.,-1.));
#9015=DIRECTION('center_axis',(0.,-1.,0.));
#9016=DIRECTION('ref_axis',(1.,0.,0.));
#9017=DIRECTION('center_axis',(0.,-1.,0.));
#9018=DIRECTION('ref_axis',(1.,0.,0.));
#9019=DIRECTION('',(0.,1.,0.));
#9020=DIRECTION('axis',(0.,0.,1.));
#9021=DIRECTION('refdir',(1.,0.,0.));
#9022=DIRECTION('center_axis',(0.,1.,0.));
#9023=DIRECTION('ref_axis',(0.,0.,1.));
#9024=DIRECTION('center_axis',(0.,-1.,0.));
#9025=DIRECTION('ref_axis',(1.,0.,0.));
#9026=DIRECTION('center_axis',(0.,-1.,0.));
#9027=DIRECTION('ref_axis',(1.,0.,0.));
#9028=DIRECTION('center_axis',(0.,-1.,0.));
#9029=DIRECTION('ref_axis',(1.,0.,0.));
#9030=DIRECTION('',(0.707106781186547,0.707106781186548,8.65956056235493E-17));
#9031=DIRECTION('center_axis',(0.,-1.,0.));
#9032=DIRECTION('ref_axis',(1.,0.,0.));
#9033=DIRECTION('center_axis',(0.,-1.,0.));
#9034=DIRECTION('ref_axis',(1.,0.,0.));
#9035=DIRECTION('',(0.,1.,0.));
#9036=DIRECTION('center_axis',(0.,1.,0.));
#9037=DIRECTION('ref_axis',(1.,0.,0.));
#9038=DIRECTION('center_axis',(0.,-1.,0.));
#9039=DIRECTION('ref_axis',(1.,0.,0.));
#9040=DIRECTION('',(-0.707106781186547,0.707106781186548,-8.65956056235493E-17));
#9041=DIRECTION('center_axis',(0.,-1.,0.));
#9042=DIRECTION('ref_axis',(0.,0.,-1.));
#9043=DIRECTION('center_axis',(0.,-1.,0.));
#9044=DIRECTION('ref_axis',(1.,0.,0.));
#9045=DIRECTION('center_axis',(0.,1.,0.));
#9046=DIRECTION('ref_axis',(1.,0.,0.));
#9047=DIRECTION('center_axis',(0.,1.,0.));
#9048=DIRECTION('ref_axis',(1.,0.,0.));
#9049=DIRECTION('',(-0.447213595499958,0.894427190999916,-5.47678698264203E-17));
#9050=DIRECTION('center_axis',(0.,-1.,0.));
#9051=DIRECTION('ref_axis',(1.,0.,0.));
#9052=DIRECTION('center_axis',(0.,1.,0.));
#9053=DIRECTION('ref_axis',(1.,0.,0.));
#9054=DIRECTION('',(0.,1.,0.));
#9055=DIRECTION('center_axis',(0.,1.,0.));
#9056=DIRECTION('ref_axis',(1.,0.,0.));
#9057=DIRECTION('center_axis',(0.,-1.,0.));
#9058=DIRECTION('ref_axis',(1.,0.,0.));
#9059=DIRECTION('',(-0.707106781186547,0.707106781186548,-8.65956056235493E-17));
#9060=DIRECTION('center_axis',(0.,-1.,0.));
#9061=DIRECTION('ref_axis',(0.,0.,-1.));
#9062=DIRECTION('center_axis',(0.866025403784439,0.,-0.5));
#9063=DIRECTION('ref_axis',(0.5,0.,0.866025403784439));
#9064=DIRECTION('',(-0.5,0.,-0.866025403784439));
#9065=DIRECTION('',(0.,-1.,0.));
#9066=DIRECTION('',(0.5,0.,0.866025403784439));
#9067=DIRECTION('',(0.,-1.,0.));
#9068=DIRECTION('center_axis',(1.60246890531964E-16,0.,-1.));
#9069=DIRECTION('ref_axis',(1.,0.,1.60246890531964E-16));
#9070=DIRECTION('',(-1.,0.,-1.60246890531964E-16));
#9071=DIRECTION('',(0.,-1.,0.));
#9072=DIRECTION('',(1.,0.,1.60246890531964E-16));
#9073=DIRECTION('center_axis',(-0.866025403784439,0.,-0.5));
#9074=DIRECTION('ref_axis',(0.5,0.,-0.866025403784439));
#9075=DIRECTION('',(-0.5,0.,0.866025403784439));
#9076=DIRECTION('',(0.,-1.,0.));
#9077=DIRECTION('',(0.5,0.,-0.866025403784439));
#9078=DIRECTION('center_axis',(-0.866025403784439,0.,0.5));
#9079=DIRECTION('ref_axis',(-0.5,0.,-0.866025403784439));
#9080=DIRECTION('',(0.5,0.,0.866025403784439));
#9081=DIRECTION('',(0.,-1.,0.));
#9082=DIRECTION('',(-0.5,0.,-0.866025403784439));
#9083=DIRECTION('center_axis',(-1.60246890531964E-16,0.,1.));
#9084=DIRECTION('ref_axis',(-1.,0.,-1.60246890531964E-16));
#9085=DIRECTION('',(1.,0.,1.60246890531964E-16));
#9086=DIRECTION('',(0.,-1.,0.));
#9087=DIRECTION('',(-1.,0.,-1.60246890531964E-16));
#9088=DIRECTION('center_axis',(0.866025403784439,0.,0.5));
#9089=DIRECTION('ref_axis',(-0.5,0.,0.866025403784439));
#9090=DIRECTION('',(0.5,0.,-0.866025403784439));
#9091=DIRECTION('',(-0.5,0.,0.866025403784439));
#9092=DIRECTION('center_axis',(0.,1.,0.));
#9093=DIRECTION('ref_axis',(1.,0.,0.));
#9094=DIRECTION('center_axis',(0.,-1.,0.));
#9095=DIRECTION('ref_axis',(0.,0.,-1.));
#9096=DIRECTION('',(0.,0.,1.));
#9097=DIRECTION('',(1.,0.,0.));
#9098=DIRECTION('',(0.,0.,1.));
#9099=DIRECTION('',(1.,0.,0.));
#9100=DIRECTION('',(0.,0.,1.));
#9101=DIRECTION('',(1.,0.,0.));
#9102=DIRECTION('',(0.,0.,1.));
#9103=DIRECTION('',(1.,0.,0.));
#9104=DIRECTION('',(0.,0.,1.));
#9105=DIRECTION('',(1.,0.,0.));
#9106=DIRECTION('',(0.,0.,1.));
#9107=DIRECTION('',(1.,0.,0.));
#9108=DIRECTION('',(0.,0.,1.));
#9109=DIRECTION('',(1.,0.,0.));
#9110=DIRECTION('',(0.,0.,1.));
#9111=DIRECTION('',(1.,0.,0.));
#9112=DIRECTION('',(0.,0.,1.));
#9113=DIRECTION('',(1.,0.,0.));
#9114=DIRECTION('',(0.,0.,1.));
#9115=DIRECTION('',(1.,0.,0.));
#9116=DIRECTION('',(0.,0.,1.));
#9117=DIRECTION('',(1.,0.,0.));
#9118=DIRECTION('',(0.,0.,1.));
#9119=DIRECTION('',(1.,0.,0.));
#9120=DIRECTION('',(0.,0.,1.));
#9121=DIRECTION('',(1.,0.,0.));
#9122=DIRECTION('',(0.,0.,1.));
#9123=DIRECTION('',(1.,0.,0.));
#9124=DIRECTION('',(0.,0.,1.));
#9125=DIRECTION('',(1.,0.,0.));
#9126=DIRECTION('',(0.,0.,1.));
#9127=DIRECTION('',(1.,0.,0.));
#9128=DIRECTION('',(0.,0.,1.));
#9129=DIRECTION('',(1.,0.,0.));
#9130=DIRECTION('',(0.,0.,1.));
#9131=DIRECTION('',(1.,0.,0.));
#9132=DIRECTION('',(0.,0.,1.));
#9133=DIRECTION('',(1.,0.,0.));
#9134=DIRECTION('',(0.,0.,1.));
#9135=DIRECTION('',(1.,0.,0.));
#9136=DIRECTION('',(0.,0.,1.));
#9137=DIRECTION('',(1.,0.,0.));
#9138=DIRECTION('',(0.,0.,1.));
#9139=DIRECTION('',(1.,0.,0.));
#9140=DIRECTION('',(0.,0.,1.));
#9141=DIRECTION('',(1.,0.,0.));
#9142=DIRECTION('',(0.,0.,1.));
#9143=DIRECTION('',(1.,0.,0.));
#9144=DIRECTION('',(0.,0.,1.));
#9145=DIRECTION('',(1.,0.,0.));
#9146=DIRECTION('',(0.,0.,1.));
#9147=DIRECTION('',(1.,0.,0.));
#9148=DIRECTION('',(0.,0.,1.));
#9149=DIRECTION('',(1.,0.,0.));
#9150=DIRECTION('',(0.,0.,1.));
#9151=DIRECTION('',(1.,0.,0.));
#9152=DIRECTION('',(0.,0.,1.));
#9153=DIRECTION('',(1.,0.,0.));
#9154=DIRECTION('',(0.,0.,1.));
#9155=DIRECTION('',(1.,0.,0.));
#9156=DIRECTION('',(0.,0.,1.));
#9157=DIRECTION('',(1.,0.,0.));
#9158=DIRECTION('',(0.,-1.,2.22044604925031E-16));
#9159=DIRECTION('',(1.,0.,0.));
#9160=DIRECTION('',(0.,-1.,2.22044604925031E-16));
#9161=DIRECTION('',(1.,0.,0.));
#9162=DIRECTION('',(0.,-1.,2.22044604925031E-16));
#9163=DIRECTION('',(1.,0.,0.));
#9164=DIRECTION('',(0.,-1.,2.22044604925031E-16));
#9165=DIRECTION('',(1.,0.,0.));
#9166=DIRECTION('',(0.,-1.,2.22044604925031E-16));
#9167=DIRECTION('',(1.,0.,0.));
#9168=DIRECTION('',(0.,-1.,2.22044604925031E-16));
#9169=DIRECTION('',(1.,0.,0.));
#9170=DIRECTION('',(0.,-1.,2.22044604925031E-16));
#9171=DIRECTION('',(1.,0.,0.));
#9172=DIRECTION('',(0.,-1.,2.22044604925031E-16));
#9173=DIRECTION('',(1.,0.,0.));
#9174=DIRECTION('',(0.,0.,1.));
#9175=DIRECTION('',(-1.,1.22464679914735E-16,0.));
#9176=DIRECTION('',(0.,0.,1.));
#9177=DIRECTION('',(-1.,1.22464679914735E-16,0.));
#9178=DIRECTION('',(0.,0.,1.));
#9179=DIRECTION('',(-1.,1.22464679914735E-16,0.));
#9180=DIRECTION('',(0.,0.,1.));
#9181=DIRECTION('',(-1.,1.22464679914735E-16,0.));
#9182=DIRECTION('',(0.,-1.,2.22044604925031E-16));
#9183=DIRECTION('',(1.,0.,0.));
#9184=DIRECTION('',(0.,-1.,2.22044604925031E-16));
#9185=DIRECTION('',(1.,0.,0.));
#9186=DIRECTION('',(0.,-1.,2.22044604925031E-16));
#9187=DIRECTION('',(1.,0.,0.));
#9188=DIRECTION('',(0.,-1.,2.22044604925031E-16));
#9189=DIRECTION('',(1.,0.,0.));
#9190=DIRECTION('',(0.,-1.,2.22044604925031E-16));
#9191=DIRECTION('',(1.,0.,0.));
#9192=CARTESIAN_POINT('',(0.,0.,0.));
#9193=CARTESIAN_POINT('',(0.,0.,0.));
#9194=CARTESIAN_POINT('Origin',(4.5,-1.8,-0.1));
#9195=CARTESIAN_POINT('',(4.29,-1.8,0.));
#9196=CARTESIAN_POINT('Origin',(4.5,-1.8,0.));
#9197=CARTESIAN_POINT('',(4.29,-1.8,0.8));
#9198=CARTESIAN_POINT('',(4.29,-1.8,-0.1));
#9199=CARTESIAN_POINT('Origin',(4.5,-1.8,0.8));
#9200=CARTESIAN_POINT('Origin',(-4.5,1.8,-0.1));
#9201=CARTESIAN_POINT('',(-4.71,1.8,0.));
#9202=CARTESIAN_POINT('Origin',(-4.5,1.8,0.));
#9203=CARTESIAN_POINT('',(-4.71,1.8,0.8));
#9204=CARTESIAN_POINT('',(-4.71,1.8,-0.1));
#9205=CARTESIAN_POINT('Origin',(-4.5,1.8,0.8));
#9206=CARTESIAN_POINT('Origin',(-4.5,-1.8,-0.1));
#9207=CARTESIAN_POINT('',(-4.71,-1.8,0.));
#9208=CARTESIAN_POINT('Origin',(-4.5,-1.8,0.));
#9209=CARTESIAN_POINT('',(-4.71,-1.8,0.8));
#9210=CARTESIAN_POINT('',(-4.71,-1.8,-0.1));
#9211=CARTESIAN_POINT('Origin',(-4.5,-1.8,0.8));
#9212=CARTESIAN_POINT('Origin',(4.5,1.8,-0.1));
#9213=CARTESIAN_POINT('',(4.29,1.8,0.));
#9214=CARTESIAN_POINT('Origin',(4.5,1.8,0.));
#9215=CARTESIAN_POINT('',(4.29,1.8,0.8));
#9216=CARTESIAN_POINT('',(4.29,1.8,-0.1));
#9217=CARTESIAN_POINT('Origin',(4.5,1.8,0.8));
#9218=CARTESIAN_POINT('Origin',(7.,3.5,0.));
#9219=CARTESIAN_POINT('',(7.,3.5,0.));
#9220=CARTESIAN_POINT('',(-7.,3.5,0.));
#9221=CARTESIAN_POINT('',(7.,3.5,0.));
#9222=CARTESIAN_POINT('',(-7.,3.5,0.8));
#9223=CARTESIAN_POINT('',(-7.,3.5,0.));
#9224=CARTESIAN_POINT('',(7.,3.5,0.8));
#9225=CARTESIAN_POINT('',(7.,3.5,0.8));
#9226=CARTESIAN_POINT('',(7.,3.5,0.));
#9227=CARTESIAN_POINT('Origin',(7.,-3.5,0.));
#9228=CARTESIAN_POINT('',(7.,-3.5,0.));
#9229=CARTESIAN_POINT('',(7.,-3.5,0.));
#9230=CARTESIAN_POINT('',(7.,-3.5,0.8));
#9231=CARTESIAN_POINT('',(7.,-3.5,0.8));
#9232=CARTESIAN_POINT('',(7.,-3.5,0.));
#9233=CARTESIAN_POINT('Origin',(-7.,-3.5,0.));
#9234=CARTESIAN_POINT('',(-7.,-3.5,0.));
#9235=CARTESIAN_POINT('',(-7.,-3.5,0.));
#9236=CARTESIAN_POINT('',(-7.,-3.5,0.8));
#9237=CARTESIAN_POINT('',(-7.,-3.5,0.8));
#9238=CARTESIAN_POINT('',(-7.,-3.5,0.));
#9239=CARTESIAN_POINT('Origin',(-7.,3.5,0.));
#9240=CARTESIAN_POINT('',(-7.,3.5,0.));
#9241=CARTESIAN_POINT('',(-7.,3.5,0.8));
#9242=CARTESIAN_POINT('Origin',(0.,0.,0.8));
#9243=CARTESIAN_POINT('Origin',(0.,0.,0.));
#9244=CARTESIAN_POINT('',(0.,0.,0.));
#9245=CARTESIAN_POINT('Origin',(-4.8,0.,2.));
#9246=CARTESIAN_POINT('',(-4.965,-2.02066721859313E-17,2.));
#9247=CARTESIAN_POINT('Origin',(-4.8,0.,2.));
#9248=CARTESIAN_POINT('',(-4.965,2.02066721859313E-17,3.));
#9249=CARTESIAN_POINT('',(-4.965,-2.02066721859313E-17,2.));
#9250=CARTESIAN_POINT('Origin',(-4.8,0.,3.));
#9251=CARTESIAN_POINT('Origin',(-4.8,0.,2.));
#9252=CARTESIAN_POINT('Origin',(-4.5,-1.8,1.6));
#9253=CARTESIAN_POINT('',(-5.,-1.8,1.6));
#9254=CARTESIAN_POINT('Origin',(-4.5,-1.8,1.6));
#9255=CARTESIAN_POINT('',(-5.,-1.8,3.));
#9256=CARTESIAN_POINT('',(-5.,-1.8,1.6));
#9257=CARTESIAN_POINT('Origin',(-4.5,-1.8,3.));
#9258=CARTESIAN_POINT('Origin',(-4.5,-1.8,1.6));
#9259=CARTESIAN_POINT('',(-4.775,-1.8,1.6));
#9260=CARTESIAN_POINT('Origin',(-4.5,-1.8,1.6));
#9261=CARTESIAN_POINT('Origin',(-4.5,1.8,1.6));
#9262=CARTESIAN_POINT('',(-5.,1.8,1.6));
#9263=CARTESIAN_POINT('Origin',(-4.5,1.8,1.6));
#9264=CARTESIAN_POINT('',(-5.,1.8,3.));
#9265=CARTESIAN_POINT('',(-5.,1.8,1.6));
#9266=CARTESIAN_POINT('Origin',(-4.5,1.8,3.));
#9267=CARTESIAN_POINT('Origin',(-4.5,1.8,1.6));
#9268=CARTESIAN_POINT('',(-4.775,1.8,1.6));
#9269=CARTESIAN_POINT('Origin',(-4.5,1.8,1.6));
#9270=CARTESIAN_POINT('Origin',(-4.5,-1.8,0.7));
#9271=CARTESIAN_POINT('',(-4.775,-1.8,0.8));
#9272=CARTESIAN_POINT('Origin',(-4.5,-1.8,0.8));
#9273=CARTESIAN_POINT('',(-4.775,-1.8,0.7));
#9274=CARTESIAN_POINT('Origin',(-4.5,1.8,0.7));
#9275=CARTESIAN_POINT('',(-4.775,1.8,0.8));
#9276=CARTESIAN_POINT('Origin',(-4.5,1.8,0.8));
#9277=CARTESIAN_POINT('',(-4.775,1.8,0.7));
#9278=CARTESIAN_POINT('Origin',(-3.5,2.5,0.8));
#9279=CARTESIAN_POINT('',(-3.5,2.5,0.8));
#9280=CARTESIAN_POINT('',(-5.5,2.5,0.8));
#9281=CARTESIAN_POINT('',(-3.5,2.5,0.8));
#9282=CARTESIAN_POINT('',(-5.5,2.5,3.));
#9283=CARTESIAN_POINT('',(-5.5,2.5,0.8));
#9284=CARTESIAN_POINT('',(-3.5,2.5,3.));
#9285=CARTESIAN_POINT('',(-3.5,2.5,3.));
#9286=CARTESIAN_POINT('',(-3.5,2.5,0.8));
#9287=CARTESIAN_POINT('Origin',(-3.5,-2.5,0.8));
#9288=CARTESIAN_POINT('',(-3.5,-2.5,0.8));
#9289=CARTESIAN_POINT('',(-3.5,-2.5,0.8));
#9290=CARTESIAN_POINT('',(-3.5,-2.5,3.));
#9291=CARTESIAN_POINT('',(-3.5,-2.5,3.));
#9292=CARTESIAN_POINT('',(-3.5,-2.5,0.8));
#9293=CARTESIAN_POINT('Origin',(-5.5,-2.5,0.8));
#9294=CARTESIAN_POINT('',(-5.5,-2.5,0.8));
#9295=CARTESIAN_POINT('',(-5.5,-2.5,0.8));
#9296=CARTESIAN_POINT('',(-5.5,-2.5,3.));
#9297=CARTESIAN_POINT('',(-5.5,-2.5,3.));
#9298=CARTESIAN_POINT('',(-5.5,-2.5,0.8));
#9299=CARTESIAN_POINT('Origin',(-5.5,2.5,0.8));
#9300=CARTESIAN_POINT('',(-5.5,2.5,0.8));
#9301=CARTESIAN_POINT('',(-5.5,2.5,3.));
#9302=CARTESIAN_POINT('Origin',(-4.5,0.,3.));
#9303=CARTESIAN_POINT('Origin',(-4.5,0.,0.8));
#9304=CARTESIAN_POINT('',(0.,0.,0.));
#9305=CARTESIAN_POINT('Origin',(4.8,0.,2.));
#9306=CARTESIAN_POINT('',(4.635,-2.02066721859313E-17,2.));
#9307=CARTESIAN_POINT('Origin',(4.8,0.,2.));
#9308=CARTESIAN_POINT('',(4.635,2.02066721859313E-17,3.));
#9309=CARTESIAN_POINT('',(4.635,-2.02066721859313E-17,2.));
#9310=CARTESIAN_POINT('Origin',(4.8,0.,3.));
#9311=CARTESIAN_POINT('Origin',(4.8,0.,2.));
#9312=CARTESIAN_POINT('Origin',(4.5,-1.8,1.6));
#9313=CARTESIAN_POINT('',(4.,-1.8,1.6));
#9314=CARTESIAN_POINT('Origin',(4.5,-1.8,1.6));
#9315=CARTESIAN_POINT('',(4.,-1.8,3.));
#9316=CARTESIAN_POINT('',(4.,-1.8,1.6));
#9317=CARTESIAN_POINT('Origin',(4.5,-1.8,3.));
#9318=CARTESIAN_POINT('Origin',(4.5,-1.8,1.6));
#9319=CARTESIAN_POINT('',(4.225,-1.8,1.6));
#9320=CARTESIAN_POINT('Origin',(4.5,-1.8,1.6));
#9321=CARTESIAN_POINT('Origin',(4.5,1.8,1.6));
#9322=CARTESIAN_POINT('',(4.,1.8,1.6));
#9323=CARTESIAN_POINT('Origin',(4.5,1.8,1.6));
#9324=CARTESIAN_POINT('',(4.,1.8,3.));
#9325=CARTESIAN_POINT('',(4.,1.8,1.6));
#9326=CARTESIAN_POINT('Origin',(4.5,1.8,3.));
#9327=CARTESIAN_POINT('Origin',(4.5,1.8,1.6));
#9328=CARTESIAN_POINT('',(4.225,1.8,1.6));
#9329=CARTESIAN_POINT('Origin',(4.5,1.8,1.6));
#9330=CARTESIAN_POINT('Origin',(4.5,-1.8,0.7));
#9331=CARTESIAN_POINT('',(4.225,-1.8,0.8));
#9332=CARTESIAN_POINT('Origin',(4.5,-1.8,0.8));
#9333=CARTESIAN_POINT('',(4.225,-1.8,0.7));
#9334=CARTESIAN_POINT('Origin',(4.5,1.8,0.7));
#9335=CARTESIAN_POINT('',(4.225,1.8,0.8));
#9336=CARTESIAN_POINT('Origin',(4.5,1.8,0.8));
#9337=CARTESIAN_POINT('',(4.225,1.8,0.7));
#9338=CARTESIAN_POINT('Origin',(5.5,2.5,0.8));
#9339=CARTESIAN_POINT('',(5.5,2.5,0.8));
#9340=CARTESIAN_POINT('',(3.5,2.5,0.8));
#9341=CARTESIAN_POINT('',(5.5,2.5,0.8));
#9342=CARTESIAN_POINT('',(3.5,2.5,3.));
#9343=CARTESIAN_POINT('',(3.5,2.5,0.8));
#9344=CARTESIAN_POINT('',(5.5,2.5,3.));
#9345=CARTESIAN_POINT('',(5.5,2.5,3.));
#9346=CARTESIAN_POINT('',(5.5,2.5,0.8));
#9347=CARTESIAN_POINT('Origin',(5.5,-2.5,0.8));
#9348=CARTESIAN_POINT('',(5.5,-2.5,0.8));
#9349=CARTESIAN_POINT('',(5.5,-2.5,0.8));
#9350=CARTESIAN_POINT('',(5.5,-2.5,3.));
#9351=CARTESIAN_POINT('',(5.5,-2.5,3.));
#9352=CARTESIAN_POINT('',(5.5,-2.5,0.8));
#9353=CARTESIAN_POINT('Origin',(3.5,-2.5,0.8));
#9354=CARTESIAN_POINT('',(3.5,-2.5,0.8));
#9355=CARTESIAN_POINT('',(3.5,-2.5,0.8));
#9356=CARTESIAN_POINT('',(3.5,-2.5,3.));
#9357=CARTESIAN_POINT('',(3.5,-2.5,3.));
#9358=CARTESIAN_POINT('',(3.5,-2.5,0.8));
#9359=CARTESIAN_POINT('Origin',(3.5,2.5,0.8));
#9360=CARTESIAN_POINT('',(3.5,2.5,0.8));
#9361=CARTESIAN_POINT('',(3.5,2.5,3.));
#9362=CARTESIAN_POINT('Origin',(4.5,0.,3.));
#9363=CARTESIAN_POINT('Origin',(4.5,0.,0.8));
#9364=CARTESIAN_POINT('',(0.,0.,0.));
#9365=CARTESIAN_POINT('Origin',(0.,-0.1,4.));
#9366=CARTESIAN_POINT('',(0.387298334620742,-0.1,3.9));
#9367=CARTESIAN_POINT('',(-0.387298334620742,-0.1,3.9));
#9368=CARTESIAN_POINT('',(0.,-0.1,3.9));
#9369=CARTESIAN_POINT('Origin',(0.,-0.1,4.));
#9370=CARTESIAN_POINT('Origin',(0.,-0.1,4.));
#9371=CARTESIAN_POINT('',(0.387298334620742,-0.1,4.1));
#9372=CARTESIAN_POINT('',(0.387298334620742,-0.1,3.9));
#9373=CARTESIAN_POINT('Origin',(0.,-0.1,4.));
#9374=CARTESIAN_POINT('Origin',(0.,1.6,4.));
#9375=CARTESIAN_POINT('',(0.28284271247462,1.6,4.28284271247462));
#9376=CARTESIAN_POINT('',(-0.28284271247462,1.6,4.28284271247462));
#9377=CARTESIAN_POINT('',(-5.6,1.6,4.28284271247462));
#9378=CARTESIAN_POINT('Origin',(0.,1.6,4.));
#9379=CARTESIAN_POINT('Origin',(0.,-0.1,4.));
#9380=CARTESIAN_POINT('',(-0.387298334620742,0.0999999999999997,3.9));
#9381=CARTESIAN_POINT('',(-0.387298334620742,-0.1,3.9));
#9382=CARTESIAN_POINT('',(0.387298334620742,0.0999999999999997,3.9));
#9383=CARTESIAN_POINT('',(0.387298334620742,-0.1,3.9));
#9384=CARTESIAN_POINT('',(0.4,0.,4.));
#9385=CARTESIAN_POINT('Origin',(0.,0.,4.));
#9386=CARTESIAN_POINT('',(-0.4,0.,4.));
#9387=CARTESIAN_POINT('Origin',(0.,0.,4.));
#9388=CARTESIAN_POINT('',(-0.4,1.2,4.));
#9389=CARTESIAN_POINT('',(-0.4,-0.1,4.));
#9390=CARTESIAN_POINT('',(-0.264575131106459,1.5,4.3));
#9391=CARTESIAN_POINT('Ctrl Pts',(-0.264575131106459,1.5,4.3));
#9392=CARTESIAN_POINT('Ctrl Pts',(-0.264575131106459,1.47985532278493,4.3));
#9393=CARTESIAN_POINT('Ctrl Pts',(-0.266946656583193,1.4596364158444,4.2979507721165));
#9394=CARTESIAN_POINT('Ctrl Pts',(-0.275663470560297,1.42025634008317,4.28990486485683));
#9395=CARTESIAN_POINT('Ctrl Pts',(-0.281970270384709,1.40108570205275,4.28391288325358));
#9396=CARTESIAN_POINT('Ctrl Pts',(-0.304063569802551,1.34650091982942,4.2607687447172));
#9397=CARTESIAN_POINT('Ctrl Pts',(-0.322818652826944,1.31392187404012,4.23818594275205));
#9398=CARTESIAN_POINT('Ctrl Pts',(-0.35507155223138,1.26236205014611,4.18662611885804));
#9399=CARTESIAN_POINT('Ctrl Pts',(-0.371172434841458,1.23945139911714,4.15398235555279));
#9400=CARTESIAN_POINT('Ctrl Pts',(-0.393713960479867,1.20823419970573,4.08042925305982));
#9401=CARTESIAN_POINT('Ctrl Pts',(-0.4,1.2,4.03944194682574));
#9402=CARTESIAN_POINT('Ctrl Pts',(-0.4,1.2,4.));
#9403=CARTESIAN_POINT('Ctrl Pts',(-0.282842712474619,1.6,4.28284271247462));
#9404=CARTESIAN_POINT('Ctrl Pts',(-0.278258894172667,1.58703500397985,4.28742653077657));
#9405=CARTESIAN_POINT('Ctrl Pts',(-0.274318439164033,1.57366719225041,4.29114637326852));
#9406=CARTESIAN_POINT('Ctrl Pts',(-0.266946656583193,1.5403635841556,4.2979507721165));
#9407=CARTESIAN_POINT('Ctrl Pts',(-0.264575131106459,1.52014467721507,4.3));
#9408=CARTESIAN_POINT('Ctrl Pts',(-0.264575131106459,1.5,4.3));
#9409=CARTESIAN_POINT('',(0.264575131106459,1.5,4.3));
#9410=CARTESIAN_POINT('Ctrl Pts',(0.264575131106459,1.5,4.3));
#9411=CARTESIAN_POINT('Ctrl Pts',(0.264575131106459,1.52014467721507,4.3));
#9412=CARTESIAN_POINT('Ctrl Pts',(0.266946656583193,1.5403635841556,4.2979507721165));
#9413=CARTESIAN_POINT('Ctrl Pts',(0.27431843921387,1.57366719247556,4.29114637322252));
#9414=CARTESIAN_POINT('Ctrl Pts',(0.278258894077422,1.58703500371046,4.28742653087182));
#9415=CARTESIAN_POINT('Ctrl Pts',(0.282842712474619,1.6,4.28284271247462));
#9416=CARTESIAN_POINT('',(0.282842712474619,1.6,3.71715728752538));
#9417=CARTESIAN_POINT('Ctrl Pts',(0.282842712474619,1.6,3.71715728752538));
#9418=CARTESIAN_POINT('Ctrl Pts',(0.278258894172666,1.58703500397985,3.71257346922343));
#9419=CARTESIAN_POINT('Ctrl Pts',(0.274318439164033,1.57366719225041,3.70885362673148));
#9420=CARTESIAN_POINT('Ctrl Pts',(0.266946656583194,1.5403635841556,3.7020492278835));
#9421=CARTESIAN_POINT('Ctrl Pts',(0.264575131106459,1.52014467721507,3.7));
#9422=CARTESIAN_POINT('Ctrl Pts',(0.264575131106459,1.5,3.7));
#9423=CARTESIAN_POINT('Ctrl Pts',(0.264575131106459,1.47985532278493,3.7));
#9424=CARTESIAN_POINT('Ctrl Pts',(0.266946656583194,1.4596364158444,3.7020492278835));
#9425=CARTESIAN_POINT('Ctrl Pts',(0.275663470560297,1.42025634008317,3.71009513514317));
#9426=CARTESIAN_POINT('Ctrl Pts',(0.281970270384708,1.40108570205275,3.71608711674642));
#9427=CARTESIAN_POINT('Ctrl Pts',(0.304063569802551,1.34650091982942,3.7392312552828));
#9428=CARTESIAN_POINT('Ctrl Pts',(0.322818652826944,1.31392187404012,3.76181405724795));
#9429=CARTESIAN_POINT('Ctrl Pts',(0.355071552231379,1.26236205014611,3.81337388114196));
#9430=CARTESIAN_POINT('Ctrl Pts',(0.371172434841458,1.23945139911714,3.84601764444721));
#9431=CARTESIAN_POINT('Ctrl Pts',(0.393713960479867,1.20823419970573,3.91957074694018));
#9432=CARTESIAN_POINT('Ctrl Pts',(0.4,1.2,3.96055805317426));
#9433=CARTESIAN_POINT('Ctrl Pts',(0.4,1.2,4.03944194682574));
#9434=CARTESIAN_POINT('Ctrl Pts',(0.393713960479867,1.20823419970573,4.08042925305982));
#9435=CARTESIAN_POINT('Ctrl Pts',(0.371172434841458,1.23945139911714,4.15398235555279));
#9436=CARTESIAN_POINT('Ctrl Pts',(0.35507155223138,1.26236205014611,4.18662611885804));
#9437=CARTESIAN_POINT('Ctrl Pts',(0.322818652826944,1.31392187404012,4.23818594275205));
#9438=CARTESIAN_POINT('Ctrl Pts',(0.304063569802551,1.34650091982942,4.2607687447172));
#9439=CARTESIAN_POINT('Ctrl Pts',(0.281970270384709,1.40108570205275,4.28391288325358));
#9440=CARTESIAN_POINT('Ctrl Pts',(0.275663470560297,1.42025634008317,4.28990486485683));
#9441=CARTESIAN_POINT('Ctrl Pts',(0.266946656583193,1.4596364158444,4.2979507721165));
#9442=CARTESIAN_POINT('Ctrl Pts',(0.264575131106459,1.47985532278493,4.3));
#9443=CARTESIAN_POINT('Ctrl Pts',(0.264575131106459,1.5,4.3));
#9444=CARTESIAN_POINT('',(-0.282842712474619,1.6,3.71715728752538));
#9445=CARTESIAN_POINT('Origin',(0.,1.6,4.));
#9446=CARTESIAN_POINT('Ctrl Pts',(-0.4,1.2,4.));
#9447=CARTESIAN_POINT('Ctrl Pts',(-0.4,1.2,3.96055805317426));
#9448=CARTESIAN_POINT('Ctrl Pts',(-0.393713960479867,1.20823419970573,3.91957074694018));
#9449=CARTESIAN_POINT('Ctrl Pts',(-0.371172434841458,1.23945139911714,3.84601764444721));
#9450=CARTESIAN_POINT('Ctrl Pts',(-0.355071552231379,1.26236205014611,3.81337388114196));
#9451=CARTESIAN_POINT('Ctrl Pts',(-0.322818652826944,1.31392187404012,3.76181405724795));
#9452=CARTESIAN_POINT('Ctrl Pts',(-0.30406356980255,1.34650091982942,3.7392312552828));
#9453=CARTESIAN_POINT('Ctrl Pts',(-0.281970270384708,1.40108570205275,3.71608711674642));
#9454=CARTESIAN_POINT('Ctrl Pts',(-0.275663470560297,1.42025634008317,3.71009513514317));
#9455=CARTESIAN_POINT('Ctrl Pts',(-0.266946656583194,1.4596364158444,3.7020492278835));
#9456=CARTESIAN_POINT('Ctrl Pts',(-0.264575131106459,1.47985532278493,3.7));
#9457=CARTESIAN_POINT('Ctrl Pts',(-0.264575131106459,1.5,3.7));
#9458=CARTESIAN_POINT('Ctrl Pts',(-0.264575131106459,1.52014467721507,3.7));
#9459=CARTESIAN_POINT('Ctrl Pts',(-0.266946656583194,1.5403635841556,3.7020492278835));
#9460=CARTESIAN_POINT('Ctrl Pts',(-0.27431843921387,1.57366719247556,3.70885362677748));
#9461=CARTESIAN_POINT('Ctrl Pts',(-0.278258894077422,1.58703500371046,3.71257346912818));
#9462=CARTESIAN_POINT('Ctrl Pts',(-0.282842712474619,1.6,3.71715728752538));
#9463=CARTESIAN_POINT('Origin',(0.,0.,4.));
#9464=CARTESIAN_POINT('Origin',(0.,-0.1,4.));
#9465=CARTESIAN_POINT('Origin',(0.,0.,4.));
#9466=CARTESIAN_POINT('Origin',(0.,0.,4.));
#9467=CARTESIAN_POINT('Origin',(0.,-0.1,4.));
#9468=CARTESIAN_POINT('',(-0.387298334620742,-0.1,4.1));
#9469=CARTESIAN_POINT('Origin',(0.,0.,4.));
#9470=CARTESIAN_POINT('Origin',(0.,-0.1,4.));
#9471=CARTESIAN_POINT('Origin',(0.,0.,4.));
#9472=CARTESIAN_POINT('Origin',(0.,1.6,4.));
#9473=CARTESIAN_POINT('',(-5.6,1.6,3.71715728752538));
#9474=CARTESIAN_POINT('Origin',(0.,-0.1,4.));
#9475=CARTESIAN_POINT('',(-0.387298334620742,-0.1,3.9));
#9476=CARTESIAN_POINT('Origin',(0.,0.,3.9));
#9477=CARTESIAN_POINT('Origin',(0.,0.,3.9));
#9478=CARTESIAN_POINT('Origin',(0.,0.,3.9));
#9479=CARTESIAN_POINT('Origin',(0.,0.,3.9));
#9480=CARTESIAN_POINT('Origin',(0.,0.,3.9));
#9481=CARTESIAN_POINT('Origin',(0.,0.,3.9));
#9482=CARTESIAN_POINT('',(-0.4,4.89858719658941E-17,4.6));
#9483=CARTESIAN_POINT('',(-0.4,-4.89858719658941E-17,3.9));
#9484=CARTESIAN_POINT('Origin',(0.,0.,4.6));
#9485=CARTESIAN_POINT('Origin',(0.,0.,3.9));
#9486=CARTESIAN_POINT('Origin',(0.,0.,3.9));
#9487=CARTESIAN_POINT('Origin',(0.,0.,3.9));
#9488=CARTESIAN_POINT('Origin',(0.,0.,4.6));
#9489=CARTESIAN_POINT('',(-0.685,-8.38883057415937E-17,4.6));
#9490=CARTESIAN_POINT('Origin',(0.,0.,4.6));
#9491=CARTESIAN_POINT('',(-0.685,8.38883057415937E-17,6.));
#9492=CARTESIAN_POINT('',(-0.685,-8.38883057415937E-17,4.6));
#9493=CARTESIAN_POINT('Origin',(0.,0.,6.));
#9494=CARTESIAN_POINT('Origin',(0.,0.,4.6));
#9495=CARTESIAN_POINT('Origin',(3.75,1.5,3.9));
#9496=CARTESIAN_POINT('',(3.75,1.35,4.25980762113533));
#9497=CARTESIAN_POINT('',(3.9,1.5,4.3));
#9498=CARTESIAN_POINT('Ctrl Pts',(3.75,1.35,4.25980762113533));
#9499=CARTESIAN_POINT('Ctrl Pts',(3.76924576004407,1.35,4.25980762113533));
#9500=CARTESIAN_POINT('Ctrl Pts',(3.78947079018949,1.35391716232849,4.26217381539294));
#9501=CARTESIAN_POINT('Ctrl Pts',(3.82628735392617,1.36931569353957,4.2701794018691));
#9502=CARTESIAN_POINT('Ctrl Pts',(3.84291866013631,1.38078662578034,4.27565507013233));
#9503=CARTESIAN_POINT('Ctrl Pts',(3.86917753388502,1.40704549952906,4.28557999151058));
#9504=CARTESIAN_POINT('Ctrl Pts',(3.88067476198869,1.42368888628284,4.29073972615592));
#9505=CARTESIAN_POINT('Ctrl Pts',(3.89609458588037,1.46055823867667,4.2979887952526));
#9506=CARTESIAN_POINT('Ctrl Pts',(3.9,1.4808067048337,4.3));
#9507=CARTESIAN_POINT('Ctrl Pts',(3.9,1.5,4.3));
#9508=CARTESIAN_POINT('',(3.6,1.5,4.3));
#9509=CARTESIAN_POINT('Ctrl Pts',(3.6,1.5,4.3));
#9510=CARTESIAN_POINT('Ctrl Pts',(3.6,1.4808067048337,4.3));
#9511=CARTESIAN_POINT('Ctrl Pts',(3.60390541411963,1.46055823867667,4.2979887952526));
#9512=CARTESIAN_POINT('Ctrl Pts',(3.61932523801131,1.42368888628284,4.29073972615592));
#9513=CARTESIAN_POINT('Ctrl Pts',(3.63082246611498,1.40704549952906,4.28557999151058));
#9514=CARTESIAN_POINT('Ctrl Pts',(3.65708133986369,1.38078662578034,4.27565507013233));
#9515=CARTESIAN_POINT('Ctrl Pts',(3.67371264607383,1.36931569353957,4.2701794018691));
#9516=CARTESIAN_POINT('Ctrl Pts',(3.71052920981051,1.35391716232849,4.26217381539294));
#9517=CARTESIAN_POINT('Ctrl Pts',(3.73075423995593,1.35,4.25980762113533));
#9518=CARTESIAN_POINT('Ctrl Pts',(3.75,1.35,4.25980762113533));
#9519=CARTESIAN_POINT('',(3.6,1.5,4.6));
#9520=CARTESIAN_POINT('',(3.6,1.5,3.9));
#9521=CARTESIAN_POINT('Origin',(3.75,1.5,4.6));
#9522=CARTESIAN_POINT('Ctrl Pts',(3.9,1.5,4.3));
#9523=CARTESIAN_POINT('Ctrl Pts',(3.9,1.5191932951663,4.3));
#9524=CARTESIAN_POINT('Ctrl Pts',(3.89609458588037,1.53944176132333,4.2979887952526));
#9525=CARTESIAN_POINT('Ctrl Pts',(3.88067476198869,1.57631111371716,4.29073972615592));
#9526=CARTESIAN_POINT('Ctrl Pts',(3.86917753388502,1.59295450047094,4.28557999151058));
#9527=CARTESIAN_POINT('Ctrl Pts',(3.84291866013631,1.61921337421966,4.27565507013233));
#9528=CARTESIAN_POINT('Ctrl Pts',(3.82628735392617,1.63068430646043,4.2701794018691));
#9529=CARTESIAN_POINT('Ctrl Pts',(3.78947079018949,1.64608283767151,4.26217381539294));
#9530=CARTESIAN_POINT('Ctrl Pts',(3.76924576004407,1.65,4.25980762113533));
#9531=CARTESIAN_POINT('Ctrl Pts',(3.73075423995593,1.65,4.25980762113533));
#9532=CARTESIAN_POINT('Ctrl Pts',(3.71052920981051,1.64608283767151,4.26217381539294));
#9533=CARTESIAN_POINT('Ctrl Pts',(3.67371264607383,1.63068430646043,4.2701794018691));
#9534=CARTESIAN_POINT('Ctrl Pts',(3.65708133986369,1.61921337421966,4.27565507013233));
#9535=CARTESIAN_POINT('Ctrl Pts',(3.63082246611498,1.59295450047094,4.28557999151058));
#9536=CARTESIAN_POINT('Ctrl Pts',(3.61932523801131,1.57631111371716,4.29073972615592));
#9537=CARTESIAN_POINT('Ctrl Pts',(3.60390541411963,1.53944176132333,4.2979887952526));
#9538=CARTESIAN_POINT('Ctrl Pts',(3.6,1.5191932951663,4.3));
#9539=CARTESIAN_POINT('Ctrl Pts',(3.6,1.5,4.3));
#9540=CARTESIAN_POINT('Origin',(3.75,1.5,4.6));
#9541=CARTESIAN_POINT('',(3.5,1.5,4.6));
#9542=CARTESIAN_POINT('Origin',(3.75,1.5,4.6));
#9543=CARTESIAN_POINT('',(3.5,1.5,6.));
#9544=CARTESIAN_POINT('',(3.5,1.5,4.6));
#9545=CARTESIAN_POINT('Origin',(3.75,1.5,6.));
#9546=CARTESIAN_POINT('Origin',(3.75,1.5,4.6));
#9547=CARTESIAN_POINT('Origin',(3.75,-1.9,4.));
#9548=CARTESIAN_POINT('',(3.55,-1.85,4.));
#9549=CARTESIAN_POINT('Origin',(3.75,-1.85,4.));
#9550=CARTESIAN_POINT('',(3.55,1.2,4.));
#9551=CARTESIAN_POINT('',(3.55,-1.9,4.));
#9552=CARTESIAN_POINT('',(3.75,1.27639320225002,4.2));
#9553=CARTESIAN_POINT('Ctrl Pts',(3.75,1.27639320225002,4.2));
#9554=CARTESIAN_POINT('Ctrl Pts',(3.72369817653558,1.27639320225002,4.2));
#9555=CARTESIAN_POINT('Ctrl Pts',(3.69666820397931,1.27127943107918,4.19456887761608));
#9556=CARTESIAN_POINT('Ctrl Pts',(3.64786664910034,1.25525524610686,4.17398313783528));
#9557=CARTESIAN_POINT('Ctrl Pts',(3.62597566474128,1.24472396775817,4.1588183772159));
#9558=CARTESIAN_POINT('Ctrl Pts',(3.59137301409757,1.22622807298917,4.12421572657219));
#9559=CARTESIAN_POINT('Ctrl Pts',(3.57608176712229,1.21683270447635,4.1022830144367));
#9560=CARTESIAN_POINT('Ctrl Pts',(3.55537554685969,1.20366430897624,4.05320424736513));
#9561=CARTESIAN_POINT('Ctrl Pts',(3.55,1.2,4.02601246699667));
#9562=CARTESIAN_POINT('Ctrl Pts',(3.55,1.2,4.));
#9563=CARTESIAN_POINT('Ctrl Pts',(3.55,1.2,4.));
#9564=CARTESIAN_POINT('Ctrl Pts',(3.55,1.2,3.97398753300333));
#9565=CARTESIAN_POINT('Ctrl Pts',(3.55537554685969,1.20366430897624,3.94679575263487));
#9566=CARTESIAN_POINT('Ctrl Pts',(3.57608176712229,1.21683270447635,3.8977169855633));
#9567=CARTESIAN_POINT('Ctrl Pts',(3.59137301409757,1.22622807298917,3.87578427342781));
#9568=CARTESIAN_POINT('Ctrl Pts',(3.62597566474128,1.24472396775817,3.8411816227841));
#9569=CARTESIAN_POINT('Ctrl Pts',(3.64786664910034,1.25525524610686,3.82601686216472));
#9570=CARTESIAN_POINT('Ctrl Pts',(3.69666820397931,1.27127943107918,3.80543112238393));
#9571=CARTESIAN_POINT('Ctrl Pts',(3.72369817653558,1.27639320225002,3.8));
#9572=CARTESIAN_POINT('Ctrl Pts',(3.77630182346442,1.27639320225002,3.8));
#9573=CARTESIAN_POINT('Ctrl Pts',(3.80333179602069,1.27127943107918,3.80543112238393));
#9574=CARTESIAN_POINT('Ctrl Pts',(3.85213335089966,1.25525524610686,3.82601686216472));
#9575=CARTESIAN_POINT('Ctrl Pts',(3.87402433525872,1.24472396775817,3.8411816227841));
#9576=CARTESIAN_POINT('Ctrl Pts',(3.90862698590243,1.22622807298917,3.87578427342781));
#9577=CARTESIAN_POINT('Ctrl Pts',(3.92391823287771,1.21683270447635,3.8977169855633));
#9578=CARTESIAN_POINT('Ctrl Pts',(3.94462445314031,1.20366430897624,3.94679575263487));
#9579=CARTESIAN_POINT('Ctrl Pts',(3.95,1.2,3.97398753300333));
#9580=CARTESIAN_POINT('Ctrl Pts',(3.95,1.2,4.02601246699667));
#9581=CARTESIAN_POINT('Ctrl Pts',(3.94462445314031,1.20366430897624,4.05320424736513));
#9582=CARTESIAN_POINT('Ctrl Pts',(3.92391823287771,1.21683270447635,4.1022830144367));
#9583=CARTESIAN_POINT('Ctrl Pts',(3.90862698590243,1.22622807298917,4.12421572657219));
#9584=CARTESIAN_POINT('Ctrl Pts',(3.87402433525872,1.24472396775817,4.1588183772159));
#9585=CARTESIAN_POINT('Ctrl Pts',(3.85213335089966,1.25525524610686,4.17398313783528));
#9586=CARTESIAN_POINT('Ctrl Pts',(3.80333179602069,1.27127943107918,4.19456887761608));
#9587=CARTESIAN_POINT('Ctrl Pts',(3.77630182346442,1.27639320225002,4.2));
#9588=CARTESIAN_POINT('Ctrl Pts',(3.75,1.27639320225002,4.2));
#9589=CARTESIAN_POINT('Origin',(3.75,-2.6,4.));
#9590=CARTESIAN_POINT('',(3.235,-2.5,4.));
#9591=CARTESIAN_POINT('Origin',(3.75,-2.5,4.));
#9592=CARTESIAN_POINT('',(3.235,-1.85,4.));
#9593=CARTESIAN_POINT('',(3.235,-2.6,4.));
#9594=CARTESIAN_POINT('Origin',(3.75,-1.85,4.));
#9595=CARTESIAN_POINT('Origin',(3.75,-1.85,4.));
#9596=CARTESIAN_POINT('Origin',(1.25,1.5,3.9));
#9597=CARTESIAN_POINT('',(1.25,1.35,4.25980762113533));
#9598=CARTESIAN_POINT('',(1.4,1.5,4.3));
#9599=CARTESIAN_POINT('Ctrl Pts',(1.25,1.35,4.25980762113533));
#9600=CARTESIAN_POINT('Ctrl Pts',(1.26924576004407,1.35,4.25980762113533));
#9601=CARTESIAN_POINT('Ctrl Pts',(1.28947079018949,1.35391716232849,4.26217381539294));
#9602=CARTESIAN_POINT('Ctrl Pts',(1.32628735392617,1.36931569353957,4.2701794018691));
#9603=CARTESIAN_POINT('Ctrl Pts',(1.34291866013631,1.38078662578034,4.27565507013233));
#9604=CARTESIAN_POINT('Ctrl Pts',(1.36917753388502,1.40704549952906,4.28557999151058));
#9605=CARTESIAN_POINT('Ctrl Pts',(1.38067476198869,1.42368888628284,4.29073972615592));
#9606=CARTESIAN_POINT('Ctrl Pts',(1.39609458588037,1.46055823867667,4.2979887952526));
#9607=CARTESIAN_POINT('Ctrl Pts',(1.4,1.4808067048337,4.3));
#9608=CARTESIAN_POINT('Ctrl Pts',(1.4,1.5,4.3));
#9609=CARTESIAN_POINT('',(1.1,1.5,4.3));
#9610=CARTESIAN_POINT('Ctrl Pts',(1.1,1.5,4.3));
#9611=CARTESIAN_POINT('Ctrl Pts',(1.1,1.4808067048337,4.3));
#9612=CARTESIAN_POINT('Ctrl Pts',(1.10390541411963,1.46055823867667,4.2979887952526));
#9613=CARTESIAN_POINT('Ctrl Pts',(1.11932523801131,1.42368888628284,4.29073972615592));
#9614=CARTESIAN_POINT('Ctrl Pts',(1.13082246611498,1.40704549952906,4.28557999151057));
#9615=CARTESIAN_POINT('Ctrl Pts',(1.15708133986369,1.38078662578034,4.27565507013233));
#9616=CARTESIAN_POINT('Ctrl Pts',(1.17371264607383,1.36931569353957,4.2701794018691));
#9617=CARTESIAN_POINT('Ctrl Pts',(1.21052920981051,1.35391716232849,4.26217381539294));
#9618=CARTESIAN_POINT('Ctrl Pts',(1.23075423995593,1.35,4.25980762113533));
#9619=CARTESIAN_POINT('Ctrl Pts',(1.25,1.35,4.25980762113533));
#9620=CARTESIAN_POINT('',(1.1,1.5,4.6));
#9621=CARTESIAN_POINT('',(1.1,1.5,3.9));
#9622=CARTESIAN_POINT('Origin',(1.25,1.5,4.6));
#9623=CARTESIAN_POINT('Ctrl Pts',(1.4,1.5,4.3));
#9624=CARTESIAN_POINT('Ctrl Pts',(1.4,1.5191932951663,4.3));
#9625=CARTESIAN_POINT('Ctrl Pts',(1.39609458588037,1.53944176132333,4.2979887952526));
#9626=CARTESIAN_POINT('Ctrl Pts',(1.38067476198869,1.57631111371716,4.29073972615592));
#9627=CARTESIAN_POINT('Ctrl Pts',(1.36917753388502,1.59295450047094,4.28557999151058));
#9628=CARTESIAN_POINT('Ctrl Pts',(1.34291866013631,1.61921337421966,4.27565507013233));
#9629=CARTESIAN_POINT('Ctrl Pts',(1.32628735392617,1.63068430646043,4.2701794018691));
#9630=CARTESIAN_POINT('Ctrl Pts',(1.28947079018949,1.64608283767151,4.26217381539294));
#9631=CARTESIAN_POINT('Ctrl Pts',(1.26924576004407,1.65,4.25980762113533));
#9632=CARTESIAN_POINT('Ctrl Pts',(1.23075423995593,1.65,4.25980762113533));
#9633=CARTESIAN_POINT('Ctrl Pts',(1.21052920981051,1.64608283767151,4.26217381539294));
#9634=CARTESIAN_POINT('Ctrl Pts',(1.17371264607383,1.63068430646043,4.2701794018691));
#9635=CARTESIAN_POINT('Ctrl Pts',(1.15708133986369,1.61921337421966,4.27565507013233));
#9636=CARTESIAN_POINT('Ctrl Pts',(1.13082246611498,1.59295450047094,4.28557999151058));
#9637=CARTESIAN_POINT('Ctrl Pts',(1.11932523801131,1.57631111371716,4.29073972615592));
#9638=CARTESIAN_POINT('Ctrl Pts',(1.10390541411963,1.53944176132333,4.2979887952526));
#9639=CARTESIAN_POINT('Ctrl Pts',(1.1,1.5191932951663,4.3));
#9640=CARTESIAN_POINT('Ctrl Pts',(1.1,1.5,4.3));
#9641=CARTESIAN_POINT('Origin',(1.25,1.5,4.6));
#9642=CARTESIAN_POINT('',(1.,1.5,4.6));
#9643=CARTESIAN_POINT('Origin',(1.25,1.5,4.6));
#9644=CARTESIAN_POINT('',(1.,1.5,6.));
#9645=CARTESIAN_POINT('',(1.,1.5,4.6));
#9646=CARTESIAN_POINT('Origin',(1.25,1.5,6.));
#9647=CARTESIAN_POINT('Origin',(1.25,1.5,4.6));
#9648=CARTESIAN_POINT('Origin',(1.25,-1.9,4.));
#9649=CARTESIAN_POINT('',(1.05,-1.85,4.));
#9650=CARTESIAN_POINT('Origin',(1.25,-1.85,4.));
#9651=CARTESIAN_POINT('',(1.05,1.2,4.));
#9652=CARTESIAN_POINT('',(1.05,-1.9,4.));
#9653=CARTESIAN_POINT('',(1.25,1.27639320225002,4.2));
#9654=CARTESIAN_POINT('Ctrl Pts',(1.25,1.27639320225002,4.2));
#9655=CARTESIAN_POINT('Ctrl Pts',(1.22369817653558,1.27639320225002,4.2));
#9656=CARTESIAN_POINT('Ctrl Pts',(1.19666820397931,1.27127943107918,4.19456887761608));
#9657=CARTESIAN_POINT('Ctrl Pts',(1.14786664910035,1.25525524610686,4.17398313783528));
#9658=CARTESIAN_POINT('Ctrl Pts',(1.12597566474129,1.24472396775817,4.1588183772159));
#9659=CARTESIAN_POINT('Ctrl Pts',(1.09137301409758,1.22622807298917,4.12421572657219));
#9660=CARTESIAN_POINT('Ctrl Pts',(1.07608176712229,1.21683270447635,4.1022830144367));
#9661=CARTESIAN_POINT('Ctrl Pts',(1.05537554685969,1.20366430897624,4.05320424736513));
#9662=CARTESIAN_POINT('Ctrl Pts',(1.05,1.2,4.02601246699667));
#9663=CARTESIAN_POINT('Ctrl Pts',(1.05,1.2,4.));
#9664=CARTESIAN_POINT('Ctrl Pts',(1.05,1.2,4.));
#9665=CARTESIAN_POINT('Ctrl Pts',(1.05,1.2,3.97398753300333));
#9666=CARTESIAN_POINT('Ctrl Pts',(1.05537554685969,1.20366430897624,3.94679575263487));
#9667=CARTESIAN_POINT('Ctrl Pts',(1.07608176712229,1.21683270447635,3.8977169855633));
#9668=CARTESIAN_POINT('Ctrl Pts',(1.09137301409758,1.22622807298917,3.87578427342781));
#9669=CARTESIAN_POINT('Ctrl Pts',(1.12597566474129,1.24472396775817,3.8411816227841));
#9670=CARTESIAN_POINT('Ctrl Pts',(1.14786664910034,1.25525524610686,3.82601686216472));
#9671=CARTESIAN_POINT('Ctrl Pts',(1.19666820397931,1.27127943107918,3.80543112238393));
#9672=CARTESIAN_POINT('Ctrl Pts',(1.22369817653558,1.27639320225002,3.8));
#9673=CARTESIAN_POINT('Ctrl Pts',(1.27630182346442,1.27639320225002,3.8));
#9674=CARTESIAN_POINT('Ctrl Pts',(1.30333179602069,1.27127943107918,3.80543112238393));
#9675=CARTESIAN_POINT('Ctrl Pts',(1.35213335089966,1.25525524610686,3.82601686216472));
#9676=CARTESIAN_POINT('Ctrl Pts',(1.37402433525871,1.24472396775817,3.8411816227841));
#9677=CARTESIAN_POINT('Ctrl Pts',(1.40862698590242,1.22622807298917,3.87578427342781));
#9678=CARTESIAN_POINT('Ctrl Pts',(1.42391823287771,1.21683270447635,3.8977169855633));
#9679=CARTESIAN_POINT('Ctrl Pts',(1.44462445314031,1.20366430897624,3.94679575263487));
#9680=CARTESIAN_POINT('Ctrl Pts',(1.45,1.2,3.97398753300333));
#9681=CARTESIAN_POINT('Ctrl Pts',(1.45,1.2,4.02601246699667));
#9682=CARTESIAN_POINT('Ctrl Pts',(1.44462445314031,1.20366430897624,4.05320424736513));
#9683=CARTESIAN_POINT('Ctrl Pts',(1.42391823287771,1.21683270447635,4.1022830144367));
#9684=CARTESIAN_POINT('Ctrl Pts',(1.40862698590242,1.22622807298917,4.12421572657219));
#9685=CARTESIAN_POINT('Ctrl Pts',(1.37402433525871,1.24472396775817,4.1588183772159));
#9686=CARTESIAN_POINT('Ctrl Pts',(1.35213335089966,1.25525524610686,4.17398313783528));
#9687=CARTESIAN_POINT('Ctrl Pts',(1.30333179602069,1.27127943107918,4.19456887761608));
#9688=CARTESIAN_POINT('Ctrl Pts',(1.27630182346442,1.27639320225002,4.2));
#9689=CARTESIAN_POINT('Ctrl Pts',(1.25,1.27639320225002,4.2));
#9690=CARTESIAN_POINT('Origin',(1.25,-2.6,4.));
#9691=CARTESIAN_POINT('',(0.735,-2.5,4.));
#9692=CARTESIAN_POINT('Origin',(1.25,-2.5,4.));
#9693=CARTESIAN_POINT('',(0.735,-1.85,4.));
#9694=CARTESIAN_POINT('',(0.735,-2.6,4.));
#9695=CARTESIAN_POINT('Origin',(1.25,-1.85,4.));
#9696=CARTESIAN_POINT('Origin',(1.25,-1.85,4.));
#9697=CARTESIAN_POINT('Origin',(-1.25,1.5,3.9));
#9698=CARTESIAN_POINT('',(-1.25,1.35,4.25980762113533));
#9699=CARTESIAN_POINT('',(-1.1,1.5,4.3));
#9700=CARTESIAN_POINT('Ctrl Pts',(-1.25,1.35,4.25980762113533));
#9701=CARTESIAN_POINT('Ctrl Pts',(-1.23075423995593,1.35,4.25980762113533));
#9702=CARTESIAN_POINT('Ctrl Pts',(-1.21052920981051,1.35391716232849,4.26217381539294));
#9703=CARTESIAN_POINT('Ctrl Pts',(-1.17371264607383,1.36931569353957,4.2701794018691));
#9704=CARTESIAN_POINT('Ctrl Pts',(-1.15708133986369,1.38078662578034,4.27565507013233));
#9705=CARTESIAN_POINT('Ctrl Pts',(-1.13082246611498,1.40704549952906,4.28557999151058));
#9706=CARTESIAN_POINT('Ctrl Pts',(-1.11932523801131,1.42368888628284,4.29073972615592));
#9707=CARTESIAN_POINT('Ctrl Pts',(-1.10390541411963,1.46055823867667,4.2979887952526));
#9708=CARTESIAN_POINT('Ctrl Pts',(-1.1,1.4808067048337,4.3));
#9709=CARTESIAN_POINT('Ctrl Pts',(-1.1,1.5,4.3));
#9710=CARTESIAN_POINT('',(-1.4,1.5,4.3));
#9711=CARTESIAN_POINT('Ctrl Pts',(-1.4,1.5,4.3));
#9712=CARTESIAN_POINT('Ctrl Pts',(-1.4,1.4808067048337,4.3));
#9713=CARTESIAN_POINT('Ctrl Pts',(-1.39609458588037,1.46055823867667,4.2979887952526));
#9714=CARTESIAN_POINT('Ctrl Pts',(-1.38067476198869,1.42368888628284,4.29073972615592));
#9715=CARTESIAN_POINT('Ctrl Pts',(-1.36917753388502,1.40704549952906,4.28557999151058));
#9716=CARTESIAN_POINT('Ctrl Pts',(-1.34291866013631,1.38078662578034,4.27565507013233));
#9717=CARTESIAN_POINT('Ctrl Pts',(-1.32628735392617,1.36931569353957,4.2701794018691));
#9718=CARTESIAN_POINT('Ctrl Pts',(-1.28947079018949,1.35391716232849,4.26217381539294));
#9719=CARTESIAN_POINT('Ctrl Pts',(-1.26924576004407,1.35,4.25980762113533));
#9720=CARTESIAN_POINT('Ctrl Pts',(-1.25,1.35,4.25980762113533));
#9721=CARTESIAN_POINT('',(-1.4,1.5,4.6));
#9722=CARTESIAN_POINT('',(-1.4,1.5,3.9));
#9723=CARTESIAN_POINT('Origin',(-1.25,1.5,4.6));
#9724=CARTESIAN_POINT('Ctrl Pts',(-1.1,1.5,4.3));
#9725=CARTESIAN_POINT('Ctrl Pts',(-1.1,1.5191932951663,4.3));
#9726=CARTESIAN_POINT('Ctrl Pts',(-1.10390541411963,1.53944176132333,4.2979887952526));
#9727=CARTESIAN_POINT('Ctrl Pts',(-1.11932523801131,1.57631111371716,4.29073972615592));
#9728=CARTESIAN_POINT('Ctrl Pts',(-1.13082246611498,1.59295450047094,4.28557999151058));
#9729=CARTESIAN_POINT('Ctrl Pts',(-1.15708133986369,1.61921337421966,4.27565507013233));
#9730=CARTESIAN_POINT('Ctrl Pts',(-1.17371264607383,1.63068430646043,4.2701794018691));
#9731=CARTESIAN_POINT('Ctrl Pts',(-1.21052920981051,1.64608283767151,4.26217381539294));
#9732=CARTESIAN_POINT('Ctrl Pts',(-1.23075423995593,1.65,4.25980762113533));
#9733=CARTESIAN_POINT('Ctrl Pts',(-1.26924576004407,1.65,4.25980762113533));
#9734=CARTESIAN_POINT('Ctrl Pts',(-1.28947079018949,1.64608283767151,4.26217381539294));
#9735=CARTESIAN_POINT('Ctrl Pts',(-1.32628735392617,1.63068430646043,4.2701794018691));
#9736=CARTESIAN_POINT('Ctrl Pts',(-1.34291866013631,1.61921337421966,4.27565507013233));
#9737=CARTESIAN_POINT('Ctrl Pts',(-1.36917753388502,1.59295450047094,4.28557999151058));
#9738=CARTESIAN_POINT('Ctrl Pts',(-1.38067476198869,1.57631111371716,4.29073972615592));
#9739=CARTESIAN_POINT('Ctrl Pts',(-1.39609458588037,1.53944176132333,4.2979887952526));
#9740=CARTESIAN_POINT('Ctrl Pts',(-1.4,1.5191932951663,4.3));
#9741=CARTESIAN_POINT('Ctrl Pts',(-1.4,1.5,4.3));
#9742=CARTESIAN_POINT('Origin',(-1.25,1.5,4.6));
#9743=CARTESIAN_POINT('',(-1.5,1.5,4.6));
#9744=CARTESIAN_POINT('Origin',(-1.25,1.5,4.6));
#9745=CARTESIAN_POINT('',(-1.5,1.5,6.));
#9746=CARTESIAN_POINT('',(-1.5,1.5,4.6));
#9747=CARTESIAN_POINT('Origin',(-1.25,1.5,6.));
#9748=CARTESIAN_POINT('Origin',(-1.25,1.5,4.6));
#9749=CARTESIAN_POINT('Origin',(-1.25,-1.9,4.));
#9750=CARTESIAN_POINT('',(-1.45,-1.85,4.));
#9751=CARTESIAN_POINT('Origin',(-1.25,-1.85,4.));
#9752=CARTESIAN_POINT('',(-1.45,1.2,4.));
#9753=CARTESIAN_POINT('',(-1.45,-1.9,4.));
#9754=CARTESIAN_POINT('',(-1.25,1.27639320225002,4.2));
#9755=CARTESIAN_POINT('Ctrl Pts',(-1.25,1.27639320225002,4.2));
#9756=CARTESIAN_POINT('Ctrl Pts',(-1.27630182346442,1.27639320225002,4.2));
#9757=CARTESIAN_POINT('Ctrl Pts',(-1.30333179602069,1.27127943107918,4.19456887761608));
#9758=CARTESIAN_POINT('Ctrl Pts',(-1.35213335089965,1.25525524610686,4.17398313783528));
#9759=CARTESIAN_POINT('Ctrl Pts',(-1.37402433525871,1.24472396775817,4.1588183772159));
#9760=CARTESIAN_POINT('Ctrl Pts',(-1.40862698590242,1.22622807298917,4.12421572657219));
#9761=CARTESIAN_POINT('Ctrl Pts',(-1.42391823287771,1.21683270447635,4.1022830144367));
#9762=CARTESIAN_POINT('Ctrl Pts',(-1.44462445314031,1.20366430897624,4.05320424736513));
#9763=CARTESIAN_POINT('Ctrl Pts',(-1.45,1.2,4.02601246699667));
#9764=CARTESIAN_POINT('Ctrl Pts',(-1.45,1.2,4.));
#9765=CARTESIAN_POINT('Ctrl Pts',(-1.45,1.2,4.));
#9766=CARTESIAN_POINT('Ctrl Pts',(-1.45,1.2,3.97398753300333));
#9767=CARTESIAN_POINT('Ctrl Pts',(-1.44462445314031,1.20366430897624,3.94679575263487));
#9768=CARTESIAN_POINT('Ctrl Pts',(-1.42391823287771,1.21683270447635,3.8977169855633));
#9769=CARTESIAN_POINT('Ctrl Pts',(-1.40862698590242,1.22622807298917,3.87578427342781));
#9770=CARTESIAN_POINT('Ctrl Pts',(-1.37402433525871,1.24472396775817,3.8411816227841));
#9771=CARTESIAN_POINT('Ctrl Pts',(-1.35213335089966,1.25525524610686,3.82601686216472));
#9772=CARTESIAN_POINT('Ctrl Pts',(-1.30333179602069,1.27127943107918,3.80543112238392));
#9773=CARTESIAN_POINT('Ctrl Pts',(-1.27630182346442,1.27639320225002,3.8));
#9774=CARTESIAN_POINT('Ctrl Pts',(-1.22369817653558,1.27639320225002,3.8));
#9775=CARTESIAN_POINT('Ctrl Pts',(-1.19666820397931,1.27127943107918,3.80543112238393));
#9776=CARTESIAN_POINT('Ctrl Pts',(-1.14786664910034,1.25525524610686,3.82601686216472));
#9777=CARTESIAN_POINT('Ctrl Pts',(-1.12597566474129,1.24472396775817,3.8411816227841));
#9778=CARTESIAN_POINT('Ctrl Pts',(-1.09137301409758,1.22622807298917,3.87578427342781));
#9779=CARTESIAN_POINT('Ctrl Pts',(-1.07608176712229,1.21683270447635,3.8977169855633));
#9780=CARTESIAN_POINT('Ctrl Pts',(-1.05537554685969,1.20366430897624,3.94679575263487));
#9781=CARTESIAN_POINT('Ctrl Pts',(-1.05,1.2,3.97398753300333));
#9782=CARTESIAN_POINT('Ctrl Pts',(-1.05,1.2,4.02601246699667));
#9783=CARTESIAN_POINT('Ctrl Pts',(-1.05537554685969,1.20366430897624,4.05320424736513));
#9784=CARTESIAN_POINT('Ctrl Pts',(-1.07608176712229,1.21683270447635,4.10228301443669));
#9785=CARTESIAN_POINT('Ctrl Pts',(-1.09137301409758,1.22622807298917,4.12421572657219));
#9786=CARTESIAN_POINT('Ctrl Pts',(-1.12597566474129,1.24472396775817,4.1588183772159));
#9787=CARTESIAN_POINT('Ctrl Pts',(-1.14786664910034,1.25525524610686,4.17398313783528));
#9788=CARTESIAN_POINT('Ctrl Pts',(-1.19666820397931,1.27127943107918,4.19456887761607));
#9789=CARTESIAN_POINT('Ctrl Pts',(-1.22369817653558,1.27639320225002,4.2));
#9790=CARTESIAN_POINT('Ctrl Pts',(-1.25,1.27639320225002,4.2));
#9791=CARTESIAN_POINT('Origin',(-1.25,-2.6,4.));
#9792=CARTESIAN_POINT('',(-1.765,-2.5,4.));
#9793=CARTESIAN_POINT('Origin',(-1.25,-2.5,4.));
#9794=CARTESIAN_POINT('',(-1.765,-1.85,4.));
#9795=CARTESIAN_POINT('',(-1.765,-2.6,4.));
#9796=CARTESIAN_POINT('Origin',(-1.25,-1.85,4.));
#9797=CARTESIAN_POINT('Origin',(-1.25,-1.85,4.));
#9798=CARTESIAN_POINT('Origin',(-3.75,1.5,3.9));
#9799=CARTESIAN_POINT('',(-3.75,1.35,4.25980762113533));
#9800=CARTESIAN_POINT('',(-3.6,1.5,4.3));
#9801=CARTESIAN_POINT('Ctrl Pts',(-3.75,1.35,4.25980762113533));
#9802=CARTESIAN_POINT('Ctrl Pts',(-3.73075423995593,1.35,4.25980762113533));
#9803=CARTESIAN_POINT('Ctrl Pts',(-3.71052920981051,1.35391716232849,4.26217381539294));
#9804=CARTESIAN_POINT('Ctrl Pts',(-3.67371264607383,1.36931569353957,4.2701794018691));
#9805=CARTESIAN_POINT('Ctrl Pts',(-3.65708133986369,1.38078662578034,4.27565507013233));
#9806=CARTESIAN_POINT('Ctrl Pts',(-3.63082246611498,1.40704549952906,4.28557999151058));
#9807=CARTESIAN_POINT('Ctrl Pts',(-3.61932523801131,1.42368888628284,4.29073972615592));
#9808=CARTESIAN_POINT('Ctrl Pts',(-3.60390541411963,1.46055823867667,4.2979887952526));
#9809=CARTESIAN_POINT('Ctrl Pts',(-3.6,1.4808067048337,4.3));
#9810=CARTESIAN_POINT('Ctrl Pts',(-3.6,1.5,4.3));
#9811=CARTESIAN_POINT('',(-3.9,1.5,4.3));
#9812=CARTESIAN_POINT('Ctrl Pts',(-3.9,1.5,4.3));
#9813=CARTESIAN_POINT('Ctrl Pts',(-3.9,1.4808067048337,4.3));
#9814=CARTESIAN_POINT('Ctrl Pts',(-3.89609458588037,1.46055823867667,4.2979887952526));
#9815=CARTESIAN_POINT('Ctrl Pts',(-3.88067476198869,1.42368888628284,4.29073972615592));
#9816=CARTESIAN_POINT('Ctrl Pts',(-3.86917753388502,1.40704549952906,4.28557999151058));
#9817=CARTESIAN_POINT('Ctrl Pts',(-3.84291866013631,1.38078662578034,4.27565507013233));
#9818=CARTESIAN_POINT('Ctrl Pts',(-3.82628735392617,1.36931569353957,4.2701794018691));
#9819=CARTESIAN_POINT('Ctrl Pts',(-3.78947079018949,1.35391716232849,4.26217381539294));
#9820=CARTESIAN_POINT('Ctrl Pts',(-3.76924576004407,1.35,4.25980762113533));
#9821=CARTESIAN_POINT('Ctrl Pts',(-3.75,1.35,4.25980762113533));
#9822=CARTESIAN_POINT('',(-3.9,1.5,4.6));
#9823=CARTESIAN_POINT('',(-3.9,1.5,3.9));
#9824=CARTESIAN_POINT('Origin',(-3.75,1.5,4.6));
#9825=CARTESIAN_POINT('Ctrl Pts',(-3.6,1.5,4.3));
#9826=CARTESIAN_POINT('Ctrl Pts',(-3.6,1.5191932951663,4.3));
#9827=CARTESIAN_POINT('Ctrl Pts',(-3.60390541411963,1.53944176132333,4.2979887952526));
#9828=CARTESIAN_POINT('Ctrl Pts',(-3.61932523801131,1.57631111371716,4.29073972615592));
#9829=CARTESIAN_POINT('Ctrl Pts',(-3.63082246611498,1.59295450047094,4.28557999151058));
#9830=CARTESIAN_POINT('Ctrl Pts',(-3.65708133986369,1.61921337421966,4.27565507013233));
#9831=CARTESIAN_POINT('Ctrl Pts',(-3.67371264607383,1.63068430646043,4.2701794018691));
#9832=CARTESIAN_POINT('Ctrl Pts',(-3.71052920981051,1.64608283767151,4.26217381539294));
#9833=CARTESIAN_POINT('Ctrl Pts',(-3.73075423995593,1.65,4.25980762113533));
#9834=CARTESIAN_POINT('Ctrl Pts',(-3.76924576004407,1.65,4.25980762113533));
#9835=CARTESIAN_POINT('Ctrl Pts',(-3.78947079018949,1.64608283767151,4.26217381539294));
#9836=CARTESIAN_POINT('Ctrl Pts',(-3.82628735392617,1.63068430646043,4.2701794018691));
#9837=CARTESIAN_POINT('Ctrl Pts',(-3.84291866013631,1.61921337421966,4.27565507013233));
#9838=CARTESIAN_POINT('Ctrl Pts',(-3.86917753388502,1.59295450047094,4.28557999151058));
#9839=CARTESIAN_POINT('Ctrl Pts',(-3.88067476198869,1.57631111371716,4.29073972615592));
#9840=CARTESIAN_POINT('Ctrl Pts',(-3.89609458588037,1.53944176132333,4.2979887952526));
#9841=CARTESIAN_POINT('Ctrl Pts',(-3.9,1.5191932951663,4.3));
#9842=CARTESIAN_POINT('Ctrl Pts',(-3.9,1.5,4.3));
#9843=CARTESIAN_POINT('Origin',(-3.75,1.5,4.6));
#9844=CARTESIAN_POINT('',(-4.,1.5,4.6));
#9845=CARTESIAN_POINT('Origin',(-3.75,1.5,4.6));
#9846=CARTESIAN_POINT('',(-4.,1.5,6.));
#9847=CARTESIAN_POINT('',(-4.,1.5,4.6));
#9848=CARTESIAN_POINT('Origin',(-3.75,1.5,6.));
#9849=CARTESIAN_POINT('Origin',(-3.75,1.5,4.6));
#9850=CARTESIAN_POINT('Origin',(-3.75,-1.9,4.));
#9851=CARTESIAN_POINT('',(-3.95,-1.85,4.));
#9852=CARTESIAN_POINT('Origin',(-3.75,-1.85,4.));
#9853=CARTESIAN_POINT('',(-3.95,1.2,4.));
#9854=CARTESIAN_POINT('',(-3.95,-1.9,4.));
#9855=CARTESIAN_POINT('',(-3.75,1.27639320225002,4.2));
#9856=CARTESIAN_POINT('Ctrl Pts',(-3.75,1.27639320225002,4.2));
#9857=CARTESIAN_POINT('Ctrl Pts',(-3.77630182346442,1.27639320225002,4.2));
#9858=CARTESIAN_POINT('Ctrl Pts',(-3.80333179602069,1.27127943107918,4.19456887761608));
#9859=CARTESIAN_POINT('Ctrl Pts',(-3.85213335089966,1.25525524610686,4.17398313783528));
#9860=CARTESIAN_POINT('Ctrl Pts',(-3.87402433525872,1.24472396775817,4.1588183772159));
#9861=CARTESIAN_POINT('Ctrl Pts',(-3.90862698590243,1.22622807298917,4.12421572657219));
#9862=CARTESIAN_POINT('Ctrl Pts',(-3.92391823287771,1.21683270447635,4.1022830144367));
#9863=CARTESIAN_POINT('Ctrl Pts',(-3.94462445314031,1.20366430897624,4.05320424736513));
#9864=CARTESIAN_POINT('Ctrl Pts',(-3.95,1.2,4.02601246699667));
#9865=CARTESIAN_POINT('Ctrl Pts',(-3.95,1.2,4.));
#9866=CARTESIAN_POINT('Ctrl Pts',(-3.95,1.2,4.));
#9867=CARTESIAN_POINT('Ctrl Pts',(-3.95,1.2,3.97398753300333));
#9868=CARTESIAN_POINT('Ctrl Pts',(-3.94462445314031,1.20366430897624,3.94679575263487));
#9869=CARTESIAN_POINT('Ctrl Pts',(-3.92391823287771,1.21683270447635,3.8977169855633));
#9870=CARTESIAN_POINT('Ctrl Pts',(-3.90862698590243,1.22622807298917,3.87578427342781));
#9871=CARTESIAN_POINT('Ctrl Pts',(-3.87402433525872,1.24472396775817,3.8411816227841));
#9872=CARTESIAN_POINT('Ctrl Pts',(-3.85213335089965,1.25525524610686,3.82601686216472));
#9873=CARTESIAN_POINT('Ctrl Pts',(-3.80333179602069,1.27127943107918,3.80543112238392));
#9874=CARTESIAN_POINT('Ctrl Pts',(-3.77630182346442,1.27639320225002,3.8));
#9875=CARTESIAN_POINT('Ctrl Pts',(-3.72369817653558,1.27639320225002,3.8));
#9876=CARTESIAN_POINT('Ctrl Pts',(-3.69666820397931,1.27127943107918,3.80543112238392));
#9877=CARTESIAN_POINT('Ctrl Pts',(-3.64786664910034,1.25525524610686,3.82601686216472));
#9878=CARTESIAN_POINT('Ctrl Pts',(-3.62597566474128,1.24472396775817,3.8411816227841));
#9879=CARTESIAN_POINT('Ctrl Pts',(-3.59137301409757,1.22622807298917,3.87578427342781));
#9880=CARTESIAN_POINT('Ctrl Pts',(-3.57608176712229,1.21683270447635,3.8977169855633));
#9881=CARTESIAN_POINT('Ctrl Pts',(-3.55537554685969,1.20366430897624,3.94679575263487));
#9882=CARTESIAN_POINT('Ctrl Pts',(-3.55,1.2,3.97398753300333));
#9883=CARTESIAN_POINT('Ctrl Pts',(-3.55,1.2,4.02601246699667));
#9884=CARTESIAN_POINT('Ctrl Pts',(-3.55537554685969,1.20366430897624,4.05320424736513));
#9885=CARTESIAN_POINT('Ctrl Pts',(-3.57608176712229,1.21683270447635,4.1022830144367));
#9886=CARTESIAN_POINT('Ctrl Pts',(-3.59137301409757,1.22622807298917,4.12421572657219));
#9887=CARTESIAN_POINT('Ctrl Pts',(-3.62597566474128,1.24472396775817,4.1588183772159));
#9888=CARTESIAN_POINT('Ctrl Pts',(-3.64786664910034,1.25525524610686,4.17398313783528));
#9889=CARTESIAN_POINT('Ctrl Pts',(-3.69666820397931,1.27127943107918,4.19456887761607));
#9890=CARTESIAN_POINT('Ctrl Pts',(-3.72369817653558,1.27639320225002,4.2));
#9891=CARTESIAN_POINT('Ctrl Pts',(-3.75,1.27639320225002,4.2));
#9892=CARTESIAN_POINT('Origin',(-3.75,-2.6,4.));
#9893=CARTESIAN_POINT('',(-4.265,-2.5,4.));
#9894=CARTESIAN_POINT('Origin',(-3.75,-2.5,4.));
#9895=CARTESIAN_POINT('',(-4.265,-1.85,4.));
#9896=CARTESIAN_POINT('',(-4.265,-2.6,4.));
#9897=CARTESIAN_POINT('Origin',(-3.75,-1.85,4.));
#9898=CARTESIAN_POINT('Origin',(-3.75,-1.85,4.));
#9899=CARTESIAN_POINT('Origin',(-5.6,1.5,4.));
#9900=CARTESIAN_POINT('',(-5.5,1.5,4.3));
#9901=CARTESIAN_POINT('Origin',(-5.5,1.5,4.));
#9902=CARTESIAN_POINT('',(-5.6,1.5,4.3));
#9903=CARTESIAN_POINT('',(-5.6,1.5,4.3));
#9904=CARTESIAN_POINT('',(-5.6,1.5,4.3));
#9905=CARTESIAN_POINT('',(-5.6,1.5,4.3));
#9906=CARTESIAN_POINT('',(-5.6,1.5,4.3));
#9907=CARTESIAN_POINT('',(5.5,1.5,4.3));
#9908=CARTESIAN_POINT('',(-5.6,1.5,4.3));
#9909=CARTESIAN_POINT('Origin',(5.5,1.5,4.));
#9910=CARTESIAN_POINT('Origin',(4.8,-1.8,3.8));
#9911=CARTESIAN_POINT('',(4.4,-1.8,3.8));
#9912=CARTESIAN_POINT('Origin',(4.8,-1.8,3.8));
#9913=CARTESIAN_POINT('',(4.4,-1.8,6.));
#9914=CARTESIAN_POINT('',(4.4,-1.8,3.8));
#9915=CARTESIAN_POINT('Origin',(4.8,-1.8,6.));
#9916=CARTESIAN_POINT('Origin',(4.8,-1.8,3.8));
#9917=CARTESIAN_POINT('',(4.575,-1.8,3.8));
#9918=CARTESIAN_POINT('Origin',(4.8,-1.8,3.8));
#9919=CARTESIAN_POINT('Origin',(-4.8,0.,3.8));
#9920=CARTESIAN_POINT('',(-5.2,-4.89858719658942E-17,3.8));
#9921=CARTESIAN_POINT('Origin',(-4.8,0.,3.8));
#9922=CARTESIAN_POINT('',(-5.2,4.89858719658942E-17,6.));
#9923=CARTESIAN_POINT('',(-5.2,-4.89858719658942E-17,3.8));
#9924=CARTESIAN_POINT('Origin',(-4.8,0.,6.));
#9925=CARTESIAN_POINT('Origin',(-4.8,0.,3.8));
#9926=CARTESIAN_POINT('',(-5.025,-2.75545529808154E-17,3.8));
#9927=CARTESIAN_POINT('Origin',(-4.8,0.,3.8));
#9928=CARTESIAN_POINT('Origin',(-4.8,-1.8,3.8));
#9929=CARTESIAN_POINT('',(-5.2,-1.8,3.8));
#9930=CARTESIAN_POINT('Origin',(-4.8,-1.8,3.8));
#9931=CARTESIAN_POINT('',(-5.2,-1.8,6.));
#9932=CARTESIAN_POINT('',(-5.2,-1.8,3.8));
#9933=CARTESIAN_POINT('Origin',(-4.8,-1.8,6.));
#9934=CARTESIAN_POINT('Origin',(-4.8,-1.8,3.8));
#9935=CARTESIAN_POINT('',(-5.025,-1.8,3.8));
#9936=CARTESIAN_POINT('Origin',(-4.8,-1.8,3.8));
#9937=CARTESIAN_POINT('Origin',(4.8,0.,3.8));
#9938=CARTESIAN_POINT('',(4.4,-4.89858719658942E-17,3.8));
#9939=CARTESIAN_POINT('Origin',(4.8,0.,3.8));
#9940=CARTESIAN_POINT('',(4.4,4.89858719658942E-17,6.));
#9941=CARTESIAN_POINT('',(4.4,-4.89858719658942E-17,3.8));
#9942=CARTESIAN_POINT('Origin',(4.8,0.,6.));
#9943=CARTESIAN_POINT('Origin',(4.8,0.,3.8));
#9944=CARTESIAN_POINT('',(4.575,-2.75545529808154E-17,3.8));
#9945=CARTESIAN_POINT('Origin',(4.8,0.,3.8));
#9946=CARTESIAN_POINT('Origin',(4.8,-1.8,2.9));
#9947=CARTESIAN_POINT('',(4.575,-1.8,3.));
#9948=CARTESIAN_POINT('Origin',(4.8,-1.8,3.));
#9949=CARTESIAN_POINT('',(4.575,-1.8,2.9));
#9950=CARTESIAN_POINT('Origin',(-4.8,0.,2.9));
#9951=CARTESIAN_POINT('',(-5.025,-2.75545529808154E-17,3.));
#9952=CARTESIAN_POINT('Origin',(-4.8,0.,3.));
#9953=CARTESIAN_POINT('',(-5.025,-2.75545529808154E-17,2.9));
#9954=CARTESIAN_POINT('Origin',(-4.8,-1.8,2.9));
#9955=CARTESIAN_POINT('',(-5.025,-1.8,3.));
#9956=CARTESIAN_POINT('Origin',(-4.8,-1.8,3.));
#9957=CARTESIAN_POINT('',(-5.025,-1.8,2.9));
#9958=CARTESIAN_POINT('Origin',(4.8,0.,2.9));
#9959=CARTESIAN_POINT('',(4.575,-2.75545529808154E-17,3.));
#9960=CARTESIAN_POINT('Origin',(4.8,0.,3.));
#9961=CARTESIAN_POINT('',(4.575,-2.75545529808154E-17,2.9));
#9962=CARTESIAN_POINT('Origin',(5.5,2.5,3.));
#9963=CARTESIAN_POINT('',(5.5,2.5,3.));
#9964=CARTESIAN_POINT('',(-5.5,2.5,3.));
#9965=CARTESIAN_POINT('',(5.5,2.5,3.));
#9966=CARTESIAN_POINT('',(-5.5,2.5,6.));
#9967=CARTESIAN_POINT('',(-5.5,2.5,3.));
#9968=CARTESIAN_POINT('',(5.5,2.5,6.));
#9969=CARTESIAN_POINT('',(5.5,2.5,6.));
#9970=CARTESIAN_POINT('',(5.5,2.5,3.));
#9971=CARTESIAN_POINT('Origin',(5.5,-2.5,3.));
#9972=CARTESIAN_POINT('',(5.5,-2.5,3.));
#9973=CARTESIAN_POINT('',(5.5,-2.5,3.));
#9974=CARTESIAN_POINT('',(5.5,-2.5,6.));
#9975=CARTESIAN_POINT('',(5.5,-2.5,6.));
#9976=CARTESIAN_POINT('',(5.5,-2.5,3.));
#9977=CARTESIAN_POINT('Origin',(-5.5,-2.5,3.));
#9978=CARTESIAN_POINT('',(-5.5,-2.5,3.));
#9979=CARTESIAN_POINT('',(-5.5,-2.5,3.));
#9980=CARTESIAN_POINT('',(-5.5,-2.5,6.));
#9981=CARTESIAN_POINT('',(-5.5,-2.5,6.));
#9982=CARTESIAN_POINT('',(-5.5,-2.5,3.));
#9983=CARTESIAN_POINT('Origin',(-5.5,2.5,3.));
#9984=CARTESIAN_POINT('',(-5.5,2.5,3.));
#9985=CARTESIAN_POINT('',(-5.5,2.5,6.));
#9986=CARTESIAN_POINT('Origin',(0.,0.,6.));
#9987=CARTESIAN_POINT('Origin',(0.,0.,3.));
#9988=CARTESIAN_POINT('',(0.,0.,0.));
#9989=CARTESIAN_POINT('Origin',(-3.75,-6.5,4.));
#9990=CARTESIAN_POINT('',(-3.95,-3.2,4.));
#9991=CARTESIAN_POINT('Origin',(-3.75,-3.2,4.));
#9992=CARTESIAN_POINT('',(-3.95,-6.5,4.));
#9993=CARTESIAN_POINT('',(-3.95,-6.5,4.));
#9994=CARTESIAN_POINT('Origin',(-3.75,-6.5,4.));
#9995=CARTESIAN_POINT('Origin',(-3.75,-6.5,4.));
#9996=CARTESIAN_POINT('',(-4.05,-3.2,4.));
#9997=CARTESIAN_POINT('Origin',(-3.75,-3.2,4.));
#9998=CARTESIAN_POINT('',(-4.05,-6.5,4.));
#9999=CARTESIAN_POINT('',(-4.05,-6.5,4.));
#10000=CARTESIAN_POINT('Origin',(-3.75,-6.5,4.));
#10001=CARTESIAN_POINT('Origin',(-3.75,-3.2,4.));
#10002=CARTESIAN_POINT('Origin',(-3.75,-6.5,4.));
#10003=CARTESIAN_POINT('',(0.,0.,0.));
#10004=CARTESIAN_POINT('Origin',(-3.75,1.5,6.1));
#10005=CARTESIAN_POINT('',(-4.35,1.5,6.1));
#10006=CARTESIAN_POINT('Origin',(-3.75,1.5,6.1));
#10007=CARTESIAN_POINT('',(-4.05,1.5,6.1));
#10008=CARTESIAN_POINT('Origin',(-3.75,1.5,6.1));
#10009=CARTESIAN_POINT('Origin',(-3.75,1.5,6.1));
#10010=CARTESIAN_POINT('',(-4.35,1.5,6.5));
#10011=CARTESIAN_POINT('Origin',(-3.75,1.5,6.5));
#10012=CARTESIAN_POINT('',(-4.35,1.5,6.1));
#10013=CARTESIAN_POINT('Origin',(-3.75,1.5,6.5));
#10014=CARTESIAN_POINT('Origin',(-3.75,1.5,4.8));
#10015=CARTESIAN_POINT('',(-4.05,1.5,4.8));
#10016=CARTESIAN_POINT('Origin',(-3.75,1.5,4.8));
#10017=CARTESIAN_POINT('',(-3.85,1.5,4.8));
#10018=CARTESIAN_POINT('Origin',(-3.75,1.5,4.8));
#10019=CARTESIAN_POINT('Origin',(-3.75,1.5,4.8));
#10020=CARTESIAN_POINT('',(-4.05,1.5,4.8));
#10021=CARTESIAN_POINT('Origin',(-3.75,1.5,4.1));
#10022=CARTESIAN_POINT('',(-3.85,1.5,4.1));
#10023=CARTESIAN_POINT('',(-3.85,1.5,4.1));
#10024=CARTESIAN_POINT('Origin',(-3.75,1.5,4.1));
#10025=CARTESIAN_POINT('Origin',(-3.75,1.5,4.1));
#10026=CARTESIAN_POINT('',(0.,0.,0.));
#10027=CARTESIAN_POINT('Origin',(-3.75,1.5,6.));
#10028=CARTESIAN_POINT('',(-4.05,1.5,6.1));
#10029=CARTESIAN_POINT('Origin',(-3.75,1.5,6.1));
#10030=CARTESIAN_POINT('',(-4.05,1.5,6.));
#10031=CARTESIAN_POINT('',(-4.05,1.5,6.));
#10032=CARTESIAN_POINT('Origin',(-3.75,1.5,6.));
#10033=CARTESIAN_POINT('Origin',(-3.75,1.5,6.));
#10034=CARTESIAN_POINT('',(-4.25,1.5,6.1));
#10035=CARTESIAN_POINT('Origin',(-3.75,1.5,6.1));
#10036=CARTESIAN_POINT('',(-4.25,1.5,6.));
#10037=CARTESIAN_POINT('',(-4.25,1.5,6.));
#10038=CARTESIAN_POINT('Origin',(-3.75,1.5,6.));
#10039=CARTESIAN_POINT('Origin',(-3.75,1.5,6.1));
#10040=CARTESIAN_POINT('Origin',(-3.75,1.5,6.));
#10041=CARTESIAN_POINT('',(0.,0.,0.));
#10042=CARTESIAN_POINT('Origin',(-1.25,-6.5,4.));
#10043=CARTESIAN_POINT('',(-1.45,-3.2,4.));
#10044=CARTESIAN_POINT('Origin',(-1.25,-3.2,4.));
#10045=CARTESIAN_POINT('',(-1.45,-6.5,4.));
#10046=CARTESIAN_POINT('',(-1.45,-6.5,4.));
#10047=CARTESIAN_POINT('Origin',(-1.25,-6.5,4.));
#10048=CARTESIAN_POINT('Origin',(-1.25,-6.5,4.));
#10049=CARTESIAN_POINT('',(-1.55,-3.2,4.));
#10050=CARTESIAN_POINT('Origin',(-1.25,-3.2,4.));
#10051=CARTESIAN_POINT('',(-1.55,-6.5,4.));
#10052=CARTESIAN_POINT('',(-1.55,-6.5,4.));
#10053=CARTESIAN_POINT('Origin',(-1.25,-6.5,4.));
#10054=CARTESIAN_POINT('Origin',(-1.25,-3.2,4.));
#10055=CARTESIAN_POINT('Origin',(-1.25,-6.5,4.));
#10056=CARTESIAN_POINT('',(0.,0.,0.));
#10057=CARTESIAN_POINT('Origin',(-1.25,1.5,6.1));
#10058=CARTESIAN_POINT('',(-1.85,1.5,6.1));
#10059=CARTESIAN_POINT('Origin',(-1.25,1.5,6.1));
#10060=CARTESIAN_POINT('',(-1.55,1.5,6.1));
#10061=CARTESIAN_POINT('Origin',(-1.25,1.5,6.1));
#10062=CARTESIAN_POINT('Origin',(-1.25,1.5,6.1));
#10063=CARTESIAN_POINT('',(-1.85,1.5,6.5));
#10064=CARTESIAN_POINT('Origin',(-1.25,1.5,6.5));
#10065=CARTESIAN_POINT('',(-1.85,1.5,6.1));
#10066=CARTESIAN_POINT('Origin',(-1.25,1.5,6.5));
#10067=CARTESIAN_POINT('Origin',(-1.25,1.5,4.8));
#10068=CARTESIAN_POINT('',(-1.55,1.5,4.8));
#10069=CARTESIAN_POINT('Origin',(-1.25,1.5,4.8));
#10070=CARTESIAN_POINT('',(-1.35,1.5,4.8));
#10071=CARTESIAN_POINT('Origin',(-1.25,1.5,4.8));
#10072=CARTESIAN_POINT('Origin',(-1.25,1.5,4.8));
#10073=CARTESIAN_POINT('',(-1.55,1.5,4.8));
#10074=CARTESIAN_POINT('Origin',(-1.25,1.5,4.1));
#10075=CARTESIAN_POINT('',(-1.35,1.5,4.1));
#10076=CARTESIAN_POINT('',(-1.35,1.5,4.1));
#10077=CARTESIAN_POINT('Origin',(-1.25,1.5,4.1));
#10078=CARTESIAN_POINT('Origin',(-1.25,1.5,4.1));
#10079=CARTESIAN_POINT('',(0.,0.,0.));
#10080=CARTESIAN_POINT('Origin',(-1.25,1.5,6.));
#10081=CARTESIAN_POINT('',(-1.55,1.5,6.1));
#10082=CARTESIAN_POINT('Origin',(-1.25,1.5,6.1));
#10083=CARTESIAN_POINT('',(-1.55,1.5,6.));
#10084=CARTESIAN_POINT('',(-1.55,1.5,6.));
#10085=CARTESIAN_POINT('Origin',(-1.25,1.5,6.));
#10086=CARTESIAN_POINT('Origin',(-1.25,1.5,6.));
#10087=CARTESIAN_POINT('',(-1.75,1.5,6.1));
#10088=CARTESIAN_POINT('Origin',(-1.25,1.5,6.1));
#10089=CARTESIAN_POINT('',(-1.75,1.5,6.));
#10090=CARTESIAN_POINT('',(-1.75,1.5,6.));
#10091=CARTESIAN_POINT('Origin',(-1.25,1.5,6.));
#10092=CARTESIAN_POINT('Origin',(-1.25,1.5,6.1));
#10093=CARTESIAN_POINT('Origin',(-1.25,1.5,6.));
#10094=CARTESIAN_POINT('',(0.,0.,0.));
#10095=CARTESIAN_POINT('Origin',(1.25,-6.5,4.));
#10096=CARTESIAN_POINT('',(1.05,-3.2,4.));
#10097=CARTESIAN_POINT('Origin',(1.25,-3.2,4.));
#10098=CARTESIAN_POINT('',(1.05,-6.5,4.));
#10099=CARTESIAN_POINT('',(1.05,-6.5,4.));
#10100=CARTESIAN_POINT('Origin',(1.25,-6.5,4.));
#10101=CARTESIAN_POINT('Origin',(1.25,-6.5,4.));
#10102=CARTESIAN_POINT('',(0.95,-3.2,4.));
#10103=CARTESIAN_POINT('Origin',(1.25,-3.2,4.));
#10104=CARTESIAN_POINT('',(0.95,-6.5,4.));
#10105=CARTESIAN_POINT('',(0.95,-6.5,4.));
#10106=CARTESIAN_POINT('Origin',(1.25,-6.5,4.));
#10107=CARTESIAN_POINT('Origin',(1.25,-3.2,4.));
#10108=CARTESIAN_POINT('Origin',(1.25,-6.5,4.));
#10109=CARTESIAN_POINT('',(0.,0.,0.));
#10110=CARTESIAN_POINT('Origin',(1.25,1.5,6.1));
#10111=CARTESIAN_POINT('',(0.65,1.5,6.1));
#10112=CARTESIAN_POINT('Origin',(1.25,1.5,6.1));
#10113=CARTESIAN_POINT('',(0.95,1.5,6.1));
#10114=CARTESIAN_POINT('Origin',(1.25,1.5,6.1));
#10115=CARTESIAN_POINT('Origin',(1.25,1.5,6.1));
#10116=CARTESIAN_POINT('',(0.65,1.5,6.5));
#10117=CARTESIAN_POINT('Origin',(1.25,1.5,6.5));
#10118=CARTESIAN_POINT('',(0.65,1.5,6.1));
#10119=CARTESIAN_POINT('Origin',(1.25,1.5,6.5));
#10120=CARTESIAN_POINT('Origin',(1.25,1.5,4.8));
#10121=CARTESIAN_POINT('',(0.95,1.5,4.8));
#10122=CARTESIAN_POINT('Origin',(1.25,1.5,4.8));
#10123=CARTESIAN_POINT('',(1.15,1.5,4.8));
#10124=CARTESIAN_POINT('Origin',(1.25,1.5,4.8));
#10125=CARTESIAN_POINT('Origin',(1.25,1.5,4.8));
#10126=CARTESIAN_POINT('',(0.95,1.5,4.8));
#10127=CARTESIAN_POINT('Origin',(1.25,1.5,4.1));
#10128=CARTESIAN_POINT('',(1.15,1.5,4.1));
#10129=CARTESIAN_POINT('',(1.15,1.5,4.1));
#10130=CARTESIAN_POINT('Origin',(1.25,1.5,4.1));
#10131=CARTESIAN_POINT('Origin',(1.25,1.5,4.1));
#10132=CARTESIAN_POINT('',(0.,0.,0.));
#10133=CARTESIAN_POINT('Origin',(1.25,1.5,6.));
#10134=CARTESIAN_POINT('',(0.95,1.5,6.1));
#10135=CARTESIAN_POINT('Origin',(1.25,1.5,6.1));
#10136=CARTESIAN_POINT('',(0.95,1.5,6.));
#10137=CARTESIAN_POINT('',(0.95,1.5,6.));
#10138=CARTESIAN_POINT('Origin',(1.25,1.5,6.));
#10139=CARTESIAN_POINT('Origin',(1.25,1.5,6.));
#10140=CARTESIAN_POINT('',(0.75,1.5,6.1));
#10141=CARTESIAN_POINT('Origin',(1.25,1.5,6.1));
#10142=CARTESIAN_POINT('',(0.75,1.5,6.));
#10143=CARTESIAN_POINT('',(0.75,1.5,6.));
#10144=CARTESIAN_POINT('Origin',(1.25,1.5,6.));
#10145=CARTESIAN_POINT('Origin',(1.25,1.5,6.1));
#10146=CARTESIAN_POINT('Origin',(1.25,1.5,6.));
#10147=CARTESIAN_POINT('',(0.,0.,0.));
#10148=CARTESIAN_POINT('Origin',(3.75,-6.5,4.));
#10149=CARTESIAN_POINT('',(3.55,-3.2,4.));
#10150=CARTESIAN_POINT('Origin',(3.75,-3.2,4.));
#10151=CARTESIAN_POINT('',(3.55,-6.5,4.));
#10152=CARTESIAN_POINT('',(3.55,-6.5,4.));
#10153=CARTESIAN_POINT('Origin',(3.75,-6.5,4.));
#10154=CARTESIAN_POINT('Origin',(3.75,-6.5,4.));
#10155=CARTESIAN_POINT('',(3.45,-3.2,4.));
#10156=CARTESIAN_POINT('Origin',(3.75,-3.2,4.));
#10157=CARTESIAN_POINT('',(3.45,-6.5,4.));
#10158=CARTESIAN_POINT('',(3.45,-6.5,4.));
#10159=CARTESIAN_POINT('Origin',(3.75,-6.5,4.));
#10160=CARTESIAN_POINT('Origin',(3.75,-3.2,4.));
#10161=CARTESIAN_POINT('Origin',(3.75,-6.5,4.));
#10162=CARTESIAN_POINT('',(0.,0.,0.));
#10163=CARTESIAN_POINT('Origin',(3.75,1.5,6.1));
#10164=CARTESIAN_POINT('',(3.15,1.5,6.1));
#10165=CARTESIAN_POINT('Origin',(3.75,1.5,6.1));
#10166=CARTESIAN_POINT('',(3.45,1.5,6.1));
#10167=CARTESIAN_POINT('Origin',(3.75,1.5,6.1));
#10168=CARTESIAN_POINT('Origin',(3.75,1.5,6.1));
#10169=CARTESIAN_POINT('',(3.15,1.5,6.5));
#10170=CARTESIAN_POINT('Origin',(3.75,1.5,6.5));
#10171=CARTESIAN_POINT('',(3.15,1.5,6.1));
#10172=CARTESIAN_POINT('Origin',(3.75,1.5,6.5));
#10173=CARTESIAN_POINT('Origin',(3.75,1.5,4.8));
#10174=CARTESIAN_POINT('',(3.45,1.5,4.8));
#10175=CARTESIAN_POINT('Origin',(3.75,1.5,4.8));
#10176=CARTESIAN_POINT('',(3.65,1.5,4.8));
#10177=CARTESIAN_POINT('Origin',(3.75,1.5,4.8));
#10178=CARTESIAN_POINT('Origin',(3.75,1.5,4.8));
#10179=CARTESIAN_POINT('',(3.45,1.5,4.8));
#10180=CARTESIAN_POINT('Origin',(3.75,1.5,4.1));
#10181=CARTESIAN_POINT('',(3.65,1.5,4.1));
#10182=CARTESIAN_POINT('',(3.65,1.5,4.1));
#10183=CARTESIAN_POINT('Origin',(3.75,1.5,4.1));
#10184=CARTESIAN_POINT('Origin',(3.75,1.5,4.1));
#10185=CARTESIAN_POINT('',(0.,0.,0.));
#10186=CARTESIAN_POINT('Origin',(3.75,1.5,6.));
#10187=CARTESIAN_POINT('',(3.45,1.5,6.1));
#10188=CARTESIAN_POINT('Origin',(3.75,1.5,6.1));
#10189=CARTESIAN_POINT('',(3.45,1.5,6.));
#10190=CARTESIAN_POINT('',(3.45,1.5,6.));
#10191=CARTESIAN_POINT('Origin',(3.75,1.5,6.));
#10192=CARTESIAN_POINT('Origin',(3.75,1.5,6.));
#10193=CARTESIAN_POINT('',(3.25,1.5,6.1));
#10194=CARTESIAN_POINT('Origin',(3.75,1.5,6.1));
#10195=CARTESIAN_POINT('',(3.25,1.5,6.));
#10196=CARTESIAN_POINT('',(3.25,1.5,6.));
#10197=CARTESIAN_POINT('Origin',(3.75,1.5,6.));
#10198=CARTESIAN_POINT('Origin',(3.75,1.5,6.1));
#10199=CARTESIAN_POINT('Origin',(3.75,1.5,6.));
#10200=CARTESIAN_POINT('',(0.,0.,0.));
#10201=CARTESIAN_POINT('Origin',(-5.5,1.5,4.));
#10202=CARTESIAN_POINT('',(-5.1,1.5,4.3));
#10203=CARTESIAN_POINT('Origin',(-5.1,1.5,4.));
#10204=CARTESIAN_POINT('',(-5.5,1.5,4.3));
#10205=CARTESIAN_POINT('',(-5.5,1.5,4.3));
#10206=CARTESIAN_POINT('Origin',(-5.5,1.5,4.));
#10207=CARTESIAN_POINT('Origin',(-5.1,1.5,4.));
#10208=CARTESIAN_POINT('Origin',(-5.5,1.5,4.));
#10209=CARTESIAN_POINT('',(0.,0.,0.));
#10210=CARTESIAN_POINT('Origin',(5.1,1.5,4.));
#10211=CARTESIAN_POINT('',(5.5,1.5,4.3));
#10212=CARTESIAN_POINT('Origin',(5.5,1.5,4.));
#10213=CARTESIAN_POINT('',(5.1,1.5,4.3));
#10214=CARTESIAN_POINT('',(5.1,1.5,4.3));
#10215=CARTESIAN_POINT('Origin',(5.1,1.5,4.));
#10216=CARTESIAN_POINT('Origin',(5.5,1.5,4.));
#10217=CARTESIAN_POINT('Origin',(5.1,1.5,4.));
#10218=CARTESIAN_POINT('',(0.,0.,0.));
#10219=CARTESIAN_POINT('Origin',(-2.75,3.36777869765522E-16,13.9));
#10220=CARTESIAN_POINT('',(-2.915,3.16571197579591E-16,13.9));
#10221=CARTESIAN_POINT('Origin',(-2.75,3.36777869765522E-16,13.9));
#10222=CARTESIAN_POINT('',(-2.915,3.56984541951453E-16,15.));
#10223=CARTESIAN_POINT('',(-2.915,3.16571197579591E-16,13.9));
#10224=CARTESIAN_POINT('Origin',(-2.75,3.36777869765522E-16,15.));
#10225=CARTESIAN_POINT('Origin',(-2.75,3.33066907387547E-16,13.9));
#10226=CARTESIAN_POINT('Origin',(1.68388934882761E-16,2.75,13.9));
#10227=CARTESIAN_POINT('',(-0.165,2.75,13.9));
#10228=CARTESIAN_POINT('Origin',(1.68388934882761E-16,2.75,13.9));
#10229=CARTESIAN_POINT('',(-0.165,2.75,15.));
#10230=CARTESIAN_POINT('',(-0.165,2.75,13.9));
#10231=CARTESIAN_POINT('Origin',(1.68388934882761E-16,2.75,15.));
#10232=CARTESIAN_POINT('Origin',(1.66533453693773E-16,2.75,13.9));
#10233=CARTESIAN_POINT('Origin',(2.75,0.,13.9));
#10234=CARTESIAN_POINT('',(2.585,-2.02066721859313E-17,13.9));
#10235=CARTESIAN_POINT('Origin',(2.75,0.,13.9));
#10236=CARTESIAN_POINT('',(2.585,2.02066721859313E-17,15.));
#10237=CARTESIAN_POINT('',(2.585,-2.02066721859313E-17,13.9));
#10238=CARTESIAN_POINT('Origin',(2.75,0.,15.));
#10239=CARTESIAN_POINT('Origin',(2.75,0.,13.9));
#10240=CARTESIAN_POINT('Origin',(-5.05166804648283E-16,-2.75,13.9));
#10241=CARTESIAN_POINT('',(-0.165,-2.75,13.9));
#10242=CARTESIAN_POINT('Origin',(-5.05166804648283E-16,-2.75,13.9));
#10243=CARTESIAN_POINT('',(-0.165,-2.75,15.));
#10244=CARTESIAN_POINT('',(-0.165,-2.75,13.9));
#10245=CARTESIAN_POINT('Origin',(-5.05166804648283E-16,-2.75,15.));
#10246=CARTESIAN_POINT('Origin',(-4.9960036108132E-16,-2.75,13.9));
#10247=CARTESIAN_POINT('Origin',(0.8,-2.6,9.8));
#10248=CARTESIAN_POINT('',(0.72,-2.5,9.8));
#10249=CARTESIAN_POINT('Origin',(0.8,-2.5,9.8));
#10250=CARTESIAN_POINT('',(0.72,-2.39407602218476,9.8));
#10251=CARTESIAN_POINT('',(0.72,-2.6,9.8));
#10252=CARTESIAN_POINT('Ctrl Pts',(0.72,-2.39407602218476,9.8));
#10253=CARTESIAN_POINT('Ctrl Pts',(0.72,-2.39407602218476,9.78998650362219));
#10254=CARTESIAN_POINT('Ctrl Pts',(0.721997829419093,-2.39347795314806,
9.77933670746212));
#10255=CARTESIAN_POINT('Ctrl Pts',(0.730021672239828,-2.39104285533446,
9.75982110231822));
#10256=CARTESIAN_POINT('Ctrl Pts',(0.736044837862985,-2.38920269063634,
9.75095451399836));
#10257=CARTESIAN_POINT('Ctrl Pts',(0.750142086204369,-2.3848153859957,9.73658705643568));
#10258=CARTESIAN_POINT('Ctrl Pts',(0.759292738749644,-2.38192864200441,
9.73029163224123));
#10259=CARTESIAN_POINT('Ctrl Pts',(0.779207514547847,-2.37548840620605,
9.72199993483929));
#10260=CARTESIAN_POINT('Ctrl Pts',(0.789969133117306,-2.37193188471924,
9.72));
#10261=CARTESIAN_POINT('Ctrl Pts',(0.810120782163592,-2.36512545840249,
9.72));
#10262=CARTESIAN_POINT('Ctrl Pts',(0.820924889571242,-2.36139662819874,
9.72203247425743));
#10263=CARTESIAN_POINT('Ctrl Pts',(0.840861824541038,-2.35437106294126,
9.73037890165789));
#10264=CARTESIAN_POINT('Ctrl Pts',(0.849995310916174,-2.35107789272744,
9.73669428134057));
#10265=CARTESIAN_POINT('Ctrl Pts',(0.864015479756631,-2.34596024152528,
9.75104732679704));
#10266=CARTESIAN_POINT('Ctrl Pts',(0.87000322488351,-2.34373901948205,9.75987236006433));
#10267=CARTESIAN_POINT('Ctrl Pts',(0.877997733074498,-2.34075590003467,
9.77933523544702));
#10268=CARTESIAN_POINT('Ctrl Pts',(0.88,-2.34,9.78997584279251));
#10269=CARTESIAN_POINT('Ctrl Pts',(0.88,-2.34,9.81002415720749));
#10270=CARTESIAN_POINT('Ctrl Pts',(0.877997733074498,-2.34075590003467,
9.82066476455298));
#10271=CARTESIAN_POINT('Ctrl Pts',(0.87000322488351,-2.34373901948205,9.84012763993567));
#10272=CARTESIAN_POINT('Ctrl Pts',(0.864015479756631,-2.34596024152528,
9.84895267320296));
#10273=CARTESIAN_POINT('Ctrl Pts',(0.849995310916174,-2.35107789272744,
9.86330571865944));
#10274=CARTESIAN_POINT('Ctrl Pts',(0.840861824541038,-2.35437106294126,
9.86962109834211));
#10275=CARTESIAN_POINT('Ctrl Pts',(0.820924889571242,-2.36139662819874,
9.87796752574257));
#10276=CARTESIAN_POINT('Ctrl Pts',(0.810120782163592,-2.36512545840249,
9.88));
#10277=CARTESIAN_POINT('Ctrl Pts',(0.789969133117306,-2.37193188471924,
9.88));
#10278=CARTESIAN_POINT('Ctrl Pts',(0.779207514547847,-2.37548840620605,
9.87800006516071));
#10279=CARTESIAN_POINT('Ctrl Pts',(0.759292738749644,-2.38192864200441,
9.86970836775877));
#10280=CARTESIAN_POINT('Ctrl Pts',(0.750142086204369,-2.3848153859957,9.86341294356432));
#10281=CARTESIAN_POINT('Ctrl Pts',(0.736044837862985,-2.38920269063634,
9.84904548600165));
#10282=CARTESIAN_POINT('Ctrl Pts',(0.730021672239828,-2.39104285533446,
9.84017889768178));
#10283=CARTESIAN_POINT('Ctrl Pts',(0.721997829419093,-2.39347795314806,
9.82066329253788));
#10284=CARTESIAN_POINT('Ctrl Pts',(0.72,-2.39407602218476,9.81001349637781));
#10285=CARTESIAN_POINT('Ctrl Pts',(0.72,-2.39407602218476,9.8));
#10286=CARTESIAN_POINT('Origin',(-0.8,-2.6,13.2));
#10287=CARTESIAN_POINT('',(-0.88,-2.5,13.2));
#10288=CARTESIAN_POINT('Origin',(-0.8,-2.5,13.2));
#10289=CARTESIAN_POINT('',(-0.88,-2.34,13.2));
#10290=CARTESIAN_POINT('',(-0.88,-2.6,13.2));
#10291=CARTESIAN_POINT('Ctrl Pts',(-0.88,-2.34,13.2));
#10292=CARTESIAN_POINT('Ctrl Pts',(-0.88,-2.34,13.1899758427925));
#10293=CARTESIAN_POINT('Ctrl Pts',(-0.877997733074498,-2.34075590003467,
13.179335235447));
#10294=CARTESIAN_POINT('Ctrl Pts',(-0.87000322488351,-2.34373901948205,
13.1598723600643));
#10295=CARTESIAN_POINT('Ctrl Pts',(-0.864015479756631,-2.34596024152528,
13.151047326797));
#10296=CARTESIAN_POINT('Ctrl Pts',(-0.849995310916174,-2.35107789272744,
13.1366942813406));
#10297=CARTESIAN_POINT('Ctrl Pts',(-0.840861824541038,-2.35437106294126,
13.1303789016579));
#10298=CARTESIAN_POINT('Ctrl Pts',(-0.820924889571242,-2.36139662819874,
13.1220324742574));
#10299=CARTESIAN_POINT('Ctrl Pts',(-0.810120782163592,-2.36512545840249,
13.12));
#10300=CARTESIAN_POINT('Ctrl Pts',(-0.789969133117306,-2.37193188471924,
13.12));
#10301=CARTESIAN_POINT('Ctrl Pts',(-0.779207514547847,-2.37548840620605,
13.1219999348393));
#10302=CARTESIAN_POINT('Ctrl Pts',(-0.759292738749644,-2.38192864200441,
13.1302916322412));
#10303=CARTESIAN_POINT('Ctrl Pts',(-0.750142086204369,-2.3848153859957,
13.1365870564357));
#10304=CARTESIAN_POINT('Ctrl Pts',(-0.736044837862985,-2.38920269063634,
13.1509545139984));
#10305=CARTESIAN_POINT('Ctrl Pts',(-0.730021672239828,-2.39104285533446,
13.1598211023182));
#10306=CARTESIAN_POINT('Ctrl Pts',(-0.721997829419093,-2.39347795314806,
13.1793367074621));
#10307=CARTESIAN_POINT('Ctrl Pts',(-0.72,-2.39407602218476,13.1899865036222));
#10308=CARTESIAN_POINT('Ctrl Pts',(-0.72,-2.39407602218476,13.2100134963778));
#10309=CARTESIAN_POINT('Ctrl Pts',(-0.721997829419093,-2.39347795314806,
13.2206632925379));
#10310=CARTESIAN_POINT('Ctrl Pts',(-0.730021672239828,-2.39104285533446,
13.2401788976818));
#10311=CARTESIAN_POINT('Ctrl Pts',(-0.736044837862985,-2.38920269063634,
13.2490454860016));
#10312=CARTESIAN_POINT('Ctrl Pts',(-0.750142086204369,-2.3848153859957,
13.2634129435643));
#10313=CARTESIAN_POINT('Ctrl Pts',(-0.759292738749644,-2.38192864200441,
13.2697083677588));
#10314=CARTESIAN_POINT('Ctrl Pts',(-0.779207514547847,-2.37548840620605,
13.2780000651607));
#10315=CARTESIAN_POINT('Ctrl Pts',(-0.789969133117306,-2.37193188471924,
13.28));
#10316=CARTESIAN_POINT('Ctrl Pts',(-0.810120782163592,-2.36512545840249,
13.28));
#10317=CARTESIAN_POINT('Ctrl Pts',(-0.820924889571242,-2.36139662819874,
13.2779675257426));
#10318=CARTESIAN_POINT('Ctrl Pts',(-0.840861824541038,-2.35437106294126,
13.2696210983421));
#10319=CARTESIAN_POINT('Ctrl Pts',(-0.849995310916174,-2.35107789272744,
13.2633057186594));
#10320=CARTESIAN_POINT('Ctrl Pts',(-0.864015479756631,-2.34596024152528,
13.248952673203));
#10321=CARTESIAN_POINT('Ctrl Pts',(-0.87000322488351,-2.34373901948205,
13.2401276399357));
#10322=CARTESIAN_POINT('Ctrl Pts',(-0.877997733074498,-2.34075590003467,
13.220664764553));
#10323=CARTESIAN_POINT('Ctrl Pts',(-0.88,-2.34,13.2100241572075));
#10324=CARTESIAN_POINT('Ctrl Pts',(-0.88,-2.34,13.2));
#10325=CARTESIAN_POINT('Origin',(-0.8,-2.6,9.8));
#10326=CARTESIAN_POINT('',(-0.88,-2.5,9.8));
#10327=CARTESIAN_POINT('Origin',(-0.8,-2.5,9.8));
#10328=CARTESIAN_POINT('',(-0.88,-2.34,9.8));
#10329=CARTESIAN_POINT('',(-0.88,-2.6,9.8));
#10330=CARTESIAN_POINT('Ctrl Pts',(-0.88,-2.34,9.8));
#10331=CARTESIAN_POINT('Ctrl Pts',(-0.88,-2.34,9.78997584279251));
#10332=CARTESIAN_POINT('Ctrl Pts',(-0.877997733074498,-2.34075590003467,
9.77933523544702));
#10333=CARTESIAN_POINT('Ctrl Pts',(-0.87000322488351,-2.34373901948205,
9.75987236006433));
#10334=CARTESIAN_POINT('Ctrl Pts',(-0.864015479756631,-2.34596024152528,
9.75104732679704));
#10335=CARTESIAN_POINT('Ctrl Pts',(-0.849995310916174,-2.35107789272744,
9.73669428134057));
#10336=CARTESIAN_POINT('Ctrl Pts',(-0.840861824541038,-2.35437106294126,
9.73037890165789));
#10337=CARTESIAN_POINT('Ctrl Pts',(-0.820924889571242,-2.36139662819874,
9.72203247425743));
#10338=CARTESIAN_POINT('Ctrl Pts',(-0.810120782163592,-2.36512545840249,
9.72));
#10339=CARTESIAN_POINT('Ctrl Pts',(-0.789969133117306,-2.37193188471924,
9.72));
#10340=CARTESIAN_POINT('Ctrl Pts',(-0.779207514547847,-2.37548840620605,
9.72199993483929));
#10341=CARTESIAN_POINT('Ctrl Pts',(-0.759292738749644,-2.38192864200441,
9.73029163224123));
#10342=CARTESIAN_POINT('Ctrl Pts',(-0.750142086204369,-2.3848153859957,
9.73658705643568));
#10343=CARTESIAN_POINT('Ctrl Pts',(-0.736044837862985,-2.38920269063634,
9.75095451399836));
#10344=CARTESIAN_POINT('Ctrl Pts',(-0.730021672239828,-2.39104285533446,
9.75982110231822));
#10345=CARTESIAN_POINT('Ctrl Pts',(-0.721997829419093,-2.39347795314806,
9.77933670746212));
#10346=CARTESIAN_POINT('Ctrl Pts',(-0.72,-2.39407602218476,9.78998650362219));
#10347=CARTESIAN_POINT('Ctrl Pts',(-0.72,-2.39407602218476,9.81001349637781));
#10348=CARTESIAN_POINT('Ctrl Pts',(-0.721997829419093,-2.39347795314806,
9.82066329253788));
#10349=CARTESIAN_POINT('Ctrl Pts',(-0.730021672239828,-2.39104285533446,
9.84017889768178));
#10350=CARTESIAN_POINT('Ctrl Pts',(-0.736044837862985,-2.38920269063634,
9.84904548600165));
#10351=CARTESIAN_POINT('Ctrl Pts',(-0.750142086204369,-2.3848153859957,
9.86341294356432));
#10352=CARTESIAN_POINT('Ctrl Pts',(-0.759292738749644,-2.38192864200441,
9.86970836775877));
#10353=CARTESIAN_POINT('Ctrl Pts',(-0.779207514547847,-2.37548840620605,
9.87800006516071));
#10354=CARTESIAN_POINT('Ctrl Pts',(-0.789969133117306,-2.37193188471924,
9.88));
#10355=CARTESIAN_POINT('Ctrl Pts',(-0.810120782163592,-2.36512545840249,
9.88));
#10356=CARTESIAN_POINT('Ctrl Pts',(-0.820924889571242,-2.36139662819874,
9.87796752574257));
#10357=CARTESIAN_POINT('Ctrl Pts',(-0.840861824541038,-2.35437106294126,
9.86962109834211));
#10358=CARTESIAN_POINT('Ctrl Pts',(-0.849995310916174,-2.35107789272744,
9.86330571865944));
#10359=CARTESIAN_POINT('Ctrl Pts',(-0.864015479756631,-2.34596024152528,
9.84895267320296));
#10360=CARTESIAN_POINT('Ctrl Pts',(-0.87000322488351,-2.34373901948205,
9.84012763993567));
#10361=CARTESIAN_POINT('Ctrl Pts',(-0.877997733074498,-2.34075590003467,
9.82066476455298));
#10362=CARTESIAN_POINT('Ctrl Pts',(-0.88,-2.34,9.81002415720748));
#10363=CARTESIAN_POINT('Ctrl Pts',(-0.88,-2.34,9.8));
#10364=CARTESIAN_POINT('Origin',(0.8,-2.6,13.2));
#10365=CARTESIAN_POINT('',(0.72,-2.5,13.2));
#10366=CARTESIAN_POINT('Origin',(0.8,-2.5,13.2));
#10367=CARTESIAN_POINT('',(0.72,-2.39407602218476,13.2));
#10368=CARTESIAN_POINT('',(0.72,-2.6,13.2));
#10369=CARTESIAN_POINT('Ctrl Pts',(0.72,-2.39407602218476,13.2));
#10370=CARTESIAN_POINT('Ctrl Pts',(0.72,-2.39407602218476,13.1899865036222));
#10371=CARTESIAN_POINT('Ctrl Pts',(0.721997829419093,-2.39347795314806,
13.1793367074621));
#10372=CARTESIAN_POINT('Ctrl Pts',(0.730021672239828,-2.39104285533446,
13.1598211023182));
#10373=CARTESIAN_POINT('Ctrl Pts',(0.736044837862985,-2.38920269063634,
13.1509545139984));
#10374=CARTESIAN_POINT('Ctrl Pts',(0.750142086204369,-2.3848153859957,13.1365870564357));
#10375=CARTESIAN_POINT('Ctrl Pts',(0.759292738749644,-2.38192864200441,
13.1302916322412));
#10376=CARTESIAN_POINT('Ctrl Pts',(0.779207514547847,-2.37548840620605,
13.1219999348393));
#10377=CARTESIAN_POINT('Ctrl Pts',(0.789969133117306,-2.37193188471924,
13.12));
#10378=CARTESIAN_POINT('Ctrl Pts',(0.810120782163592,-2.36512545840249,
13.12));
#10379=CARTESIAN_POINT('Ctrl Pts',(0.820924889571242,-2.36139662819874,
13.1220324742574));
#10380=CARTESIAN_POINT('Ctrl Pts',(0.840861824541038,-2.35437106294126,
13.1303789016579));
#10381=CARTESIAN_POINT('Ctrl Pts',(0.849995310916174,-2.35107789272744,
13.1366942813406));
#10382=CARTESIAN_POINT('Ctrl Pts',(0.864015479756631,-2.34596024152528,
13.151047326797));
#10383=CARTESIAN_POINT('Ctrl Pts',(0.87000322488351,-2.34373901948205,13.1598723600643));
#10384=CARTESIAN_POINT('Ctrl Pts',(0.877997733074498,-2.34075590003467,
13.179335235447));
#10385=CARTESIAN_POINT('Ctrl Pts',(0.88,-2.34,13.1899758427925));
#10386=CARTESIAN_POINT('Ctrl Pts',(0.88,-2.34,13.2100241572075));
#10387=CARTESIAN_POINT('Ctrl Pts',(0.877997733074498,-2.34075590003467,
13.220664764553));
#10388=CARTESIAN_POINT('Ctrl Pts',(0.87000322488351,-2.34373901948205,13.2401276399357));
#10389=CARTESIAN_POINT('Ctrl Pts',(0.864015479756631,-2.34596024152528,
13.248952673203));
#10390=CARTESIAN_POINT('Ctrl Pts',(0.849995310916174,-2.35107789272744,
13.2633057186594));
#10391=CARTESIAN_POINT('Ctrl Pts',(0.840861824541038,-2.35437106294126,
13.2696210983421));
#10392=CARTESIAN_POINT('Ctrl Pts',(0.820924889571242,-2.36139662819874,
13.2779675257426));
#10393=CARTESIAN_POINT('Ctrl Pts',(0.810120782163592,-2.36512545840249,
13.28));
#10394=CARTESIAN_POINT('Ctrl Pts',(0.789969133117306,-2.37193188471924,
13.28));
#10395=CARTESIAN_POINT('Ctrl Pts',(0.779207514547847,-2.37548840620605,
13.2780000651607));
#10396=CARTESIAN_POINT('Ctrl Pts',(0.759292738749644,-2.38192864200441,
13.2697083677588));
#10397=CARTESIAN_POINT('Ctrl Pts',(0.750142086204369,-2.3848153859957,13.2634129435643));
#10398=CARTESIAN_POINT('Ctrl Pts',(0.736044837862985,-2.38920269063634,
13.2490454860016));
#10399=CARTESIAN_POINT('Ctrl Pts',(0.730021672239828,-2.39104285533446,
13.2401788976818));
#10400=CARTESIAN_POINT('Ctrl Pts',(0.721997829419093,-2.39347795314806,
13.2206632925379));
#10401=CARTESIAN_POINT('Ctrl Pts',(0.72,-2.39407602218476,13.2100134963778));
#10402=CARTESIAN_POINT('Ctrl Pts',(0.72,-2.39407602218476,13.2));
#10403=CARTESIAN_POINT('Origin',(-0.6,-3.1,10.));
#10404=CARTESIAN_POINT('',(-0.6,-2.42693221990232,13.));
#10405=CARTESIAN_POINT('',(-0.6,-2.42693221990232,10.));
#10406=CARTESIAN_POINT('',(-0.6,-2.42693221990232,8.));
#10407=CARTESIAN_POINT('',(-0.6,-2.5,13.));
#10408=CARTESIAN_POINT('',(-0.6,-3.1,13.));
#10409=CARTESIAN_POINT('',(-0.6,-2.5,10.));
#10410=CARTESIAN_POINT('',(-0.6,-2.5,10.75));
#10411=CARTESIAN_POINT('',(-0.6,-3.1,10.));
#10412=CARTESIAN_POINT('Origin',(-0.6,-3.1,13.));
#10413=CARTESIAN_POINT('',(0.6,-2.42693221990232,13.));
#10414=CARTESIAN_POINT('',(0.,-2.5,13.));
#10415=CARTESIAN_POINT('Origin',(0.,0.,13.));
#10416=CARTESIAN_POINT('',(0.6,-2.5,13.));
#10417=CARTESIAN_POINT('',(0.6,-3.1,13.));
#10418=CARTESIAN_POINT('',(-0.3,-2.5,13.));
#10419=CARTESIAN_POINT('Origin',(0.6,-3.1,10.));
#10420=CARTESIAN_POINT('',(0.,-2.5,10.));
#10421=CARTESIAN_POINT('',(0.6,-2.42693221990232,10.));
#10422=CARTESIAN_POINT('Origin',(0.,0.,10.));
#10423=CARTESIAN_POINT('',(0.6,-2.5,10.));
#10424=CARTESIAN_POINT('',(0.3,-2.5,10.));
#10425=CARTESIAN_POINT('',(0.6,-3.1,10.));
#10426=CARTESIAN_POINT('Origin',(0.6,-3.1,10.));
#10427=CARTESIAN_POINT('Origin',(0.,0.,10.));
#10428=CARTESIAN_POINT('',(0.3,-2.5,10.));
#10429=CARTESIAN_POINT('Origin',(0.6,-3.1,13.));
#10430=CARTESIAN_POINT('',(0.6,-2.42693221990232,8.));
#10431=CARTESIAN_POINT('',(0.6,-2.5,12.25));
#10432=CARTESIAN_POINT('Origin',(-0.6,-3.1,13.));
#10433=CARTESIAN_POINT('Origin',(0.,0.,13.));
#10434=CARTESIAN_POINT('',(-0.3,-2.5,13.));
#10435=CARTESIAN_POINT('Origin',(0.,-2.5,11.5));
#10436=CARTESIAN_POINT('',(0.,-2.5,9.5));
#10437=CARTESIAN_POINT('',(0.,-2.5,8.));
#10438=CARTESIAN_POINT('',(1.,-2.5,9.5));
#10439=CARTESIAN_POINT('',(-1.,-2.5,9.5));
#10440=CARTESIAN_POINT('',(1.,-2.5,13.5));
#10441=CARTESIAN_POINT('',(1.,-2.5,9.5));
#10442=CARTESIAN_POINT('',(0.,-2.5,13.5));
#10443=CARTESIAN_POINT('',(1.,-2.5,13.5));
#10444=CARTESIAN_POINT('',(0.,-2.5,8.));
#10445=CARTESIAN_POINT('Origin',(1.,-3.1,13.5));
#10446=CARTESIAN_POINT('',(1.,-2.82842712474619,13.5));
#10447=CARTESIAN_POINT('',(1.,-2.82842712474619,9.5));
#10448=CARTESIAN_POINT('',(1.,-2.82842712474619,7.));
#10449=CARTESIAN_POINT('',(1.,-3.1,13.5));
#10450=CARTESIAN_POINT('',(1.,-3.1,9.5));
#10451=CARTESIAN_POINT('Origin',(1.,-3.1,9.5));
#10452=CARTESIAN_POINT('',(-1.,-2.82842712474619,9.5));
#10453=CARTESIAN_POINT('Origin',(0.,0.,9.5));
#10454=CARTESIAN_POINT('',(-1.,-2.5,9.5));
#10455=CARTESIAN_POINT('',(-1.,-2.5,9.5));
#10456=CARTESIAN_POINT('',(-1.,-3.1,9.5));
#10457=CARTESIAN_POINT('Origin',(-1.,-3.1,9.5));
#10458=CARTESIAN_POINT('',(-1.,-2.82842712474619,13.5));
#10459=CARTESIAN_POINT('',(-1.,-2.82842712474619,7.));
#10460=CARTESIAN_POINT('',(-1.,-2.5,13.5));
#10461=CARTESIAN_POINT('',(-1.,-2.5,13.5));
#10462=CARTESIAN_POINT('',(-1.,-3.1,13.5));
#10463=CARTESIAN_POINT('Origin',(-1.,-3.1,13.5));
#10464=CARTESIAN_POINT('Origin',(0.,0.,13.5));
#10465=CARTESIAN_POINT('',(1.,-2.5,13.5));
#10466=CARTESIAN_POINT('Origin',(0.,-2.5,11.5));
#10467=CARTESIAN_POINT('',(0.,-2.5,8.));
#10468=CARTESIAN_POINT('',(0.,-2.5,8.));
#10469=CARTESIAN_POINT('Origin',(0.,0.,6.9));
#10470=CARTESIAN_POINT('',(-0.685,-8.38883057415937E-17,7.));
#10471=CARTESIAN_POINT('Origin',(0.,0.,7.));
#10472=CARTESIAN_POINT('',(-0.685,8.38883057415937E-17,8.));
#10473=CARTESIAN_POINT('',(-0.685,-8.38883057415937E-17,6.9));
#10474=CARTESIAN_POINT('Origin',(0.,0.,8.));
#10475=CARTESIAN_POINT('Origin',(0.,0.,8.));
#10476=CARTESIAN_POINT('',(1.53080849893419E-16,-2.5,8.));
#10477=CARTESIAN_POINT('Origin',(0.,0.,8.));
#10478=CARTESIAN_POINT('',(1.53080849893419E-16,-2.5,8.));
#10479=CARTESIAN_POINT('',(1.53080849893419E-16,-2.5,15.));
#10480=CARTESIAN_POINT('',(1.53080849893419E-16,-2.5,8.));
#10481=CARTESIAN_POINT('Origin',(0.,0.,15.));
#10482=CARTESIAN_POINT('Origin',(0.,0.,8.));
#10483=CARTESIAN_POINT('Origin',(0.,0.,7.));
#10484=CARTESIAN_POINT('',(-3.,-3.67394039744206E-16,15.));
#10485=CARTESIAN_POINT('Origin',(0.,0.,15.));
#10486=CARTESIAN_POINT('',(-3.,-3.67394039744206E-16,7.));
#10487=CARTESIAN_POINT('',(-3.,-3.67394039744206E-16,7.));
#10488=CARTESIAN_POINT('Origin',(0.,0.,7.));
#10489=CARTESIAN_POINT('Origin',(0.,0.,15.));
#10490=CARTESIAN_POINT('Origin',(0.,0.,7.));
#10491=CARTESIAN_POINT('',(0.,0.,0.));
#10492=CARTESIAN_POINT('Origin',(0.8,-3.2,9.8));
#10493=CARTESIAN_POINT('',(0.68,-2.7,9.8));
#10494=CARTESIAN_POINT('Origin',(0.8,-2.7,9.8));
#10495=CARTESIAN_POINT('',(0.68,-2.5,9.8));
#10496=CARTESIAN_POINT('',(0.68,-3.2,9.8));
#10497=CARTESIAN_POINT('Origin',(0.8,-2.5,9.8));
#10498=CARTESIAN_POINT('Origin',(-0.8,-3.2,13.2));
#10499=CARTESIAN_POINT('',(-0.92,-2.7,13.2));
#10500=CARTESIAN_POINT('Origin',(-0.8,-2.7,13.2));
#10501=CARTESIAN_POINT('',(-0.92,-2.5,13.2));
#10502=CARTESIAN_POINT('',(-0.92,-3.2,13.2));
#10503=CARTESIAN_POINT('Origin',(-0.8,-2.5,13.2));
#10504=CARTESIAN_POINT('Origin',(-0.8,-3.2,9.8));
#10505=CARTESIAN_POINT('',(-0.92,-2.7,9.8));
#10506=CARTESIAN_POINT('Origin',(-0.8,-2.7,9.8));
#10507=CARTESIAN_POINT('',(-0.92,-2.5,9.8));
#10508=CARTESIAN_POINT('',(-0.92,-3.2,9.8));
#10509=CARTESIAN_POINT('Origin',(-0.8,-2.5,9.8));
#10510=CARTESIAN_POINT('Origin',(0.8,-3.2,13.2));
#10511=CARTESIAN_POINT('',(0.68,-2.7,13.2));
#10512=CARTESIAN_POINT('Origin',(0.8,-2.7,13.2));
#10513=CARTESIAN_POINT('',(0.68,-2.5,13.2));
#10514=CARTESIAN_POINT('',(0.68,-3.2,13.2));
#10515=CARTESIAN_POINT('Origin',(0.8,-2.5,13.2));
#10516=CARTESIAN_POINT('Origin',(0.6,-2.8,13.));
#10517=CARTESIAN_POINT('',(0.6,-2.5,10.));
#10518=CARTESIAN_POINT('',(0.6,-2.5,13.));
#10519=CARTESIAN_POINT('',(0.6,-2.5,11.25));
#10520=CARTESIAN_POINT('',(0.6,-2.7,10.));
#10521=CARTESIAN_POINT('',(0.6,-2.8,10.));
#10522=CARTESIAN_POINT('',(0.6,-2.7,13.));
#10523=CARTESIAN_POINT('',(0.6,-2.7,11.25));
#10524=CARTESIAN_POINT('',(0.6,-2.8,13.));
#10525=CARTESIAN_POINT('Origin',(-0.6,-2.8,13.));
#10526=CARTESIAN_POINT('',(-0.6,-2.5,13.));
#10527=CARTESIAN_POINT('',(0.2,-2.5,13.));
#10528=CARTESIAN_POINT('',(-0.6,-2.7,13.));
#10529=CARTESIAN_POINT('',(-0.8,-2.7,13.));
#10530=CARTESIAN_POINT('',(-0.6,-2.8,13.));
#10531=CARTESIAN_POINT('Origin',(-0.6,-2.8,10.));
#10532=CARTESIAN_POINT('',(-0.6,-2.5,10.));
#10533=CARTESIAN_POINT('',(-0.6,-2.5,9.75));
#10534=CARTESIAN_POINT('',(-0.6,-2.7,10.));
#10535=CARTESIAN_POINT('',(-0.6,-2.7,9.75));
#10536=CARTESIAN_POINT('',(-0.6,-2.8,10.));
#10537=CARTESIAN_POINT('Origin',(0.6,-2.8,10.));
#10538=CARTESIAN_POINT('',(0.8,-2.5,10.));
#10539=CARTESIAN_POINT('',(-0.2,-2.7,10.));
#10540=CARTESIAN_POINT('Origin',(1.,-2.5,9.5));
#10541=CARTESIAN_POINT('',(1.,-2.5,9.5));
#10542=CARTESIAN_POINT('',(-1.,-2.5,9.5));
#10543=CARTESIAN_POINT('',(1.,-2.5,9.5));
#10544=CARTESIAN_POINT('',(-1.,-2.5,13.5));
#10545=CARTESIAN_POINT('',(-1.,-2.5,9.5));
#10546=CARTESIAN_POINT('',(1.,-2.5,13.5));
#10547=CARTESIAN_POINT('',(1.,-2.5,13.5));
#10548=CARTESIAN_POINT('',(1.,-2.5,9.5));
#10549=CARTESIAN_POINT('Origin',(1.,-2.7,9.5));
#10550=CARTESIAN_POINT('',(1.,-2.7,9.5));
#10551=CARTESIAN_POINT('',(1.,-2.7,9.5));
#10552=CARTESIAN_POINT('',(1.,-2.7,13.5));
#10553=CARTESIAN_POINT('',(1.,-2.7,13.5));
#10554=CARTESIAN_POINT('',(1.,-2.7,9.5));
#10555=CARTESIAN_POINT('Origin',(-1.,-2.7,9.5));
#10556=CARTESIAN_POINT('',(-1.,-2.7,9.5));
#10557=CARTESIAN_POINT('',(-1.,-2.7,9.5));
#10558=CARTESIAN_POINT('',(-1.,-2.7,13.5));
#10559=CARTESIAN_POINT('',(-1.,-2.7,13.5));
#10560=CARTESIAN_POINT('',(-1.,-2.7,9.5));
#10561=CARTESIAN_POINT('Origin',(-1.,-2.5,9.5));
#10562=CARTESIAN_POINT('',(-1.,-2.5,9.5));
#10563=CARTESIAN_POINT('',(-1.,-2.5,13.5));
#10564=CARTESIAN_POINT('Origin',(0.,-2.6,13.5));
#10565=CARTESIAN_POINT('Origin',(0.,-2.6,9.5));
#10566=CARTESIAN_POINT('',(0.,0.,0.));
#10567=CARTESIAN_POINT('Origin',(0.8,-3.2,9.8));
#10568=CARTESIAN_POINT('',(0.68,-2.9,9.8));
#10569=CARTESIAN_POINT('Origin',(0.8,-2.9,9.8));
#10570=CARTESIAN_POINT('',(0.68,-2.7,9.8));
#10571=CARTESIAN_POINT('',(0.68,-3.2,9.8));
#10572=CARTESIAN_POINT('Origin',(0.8,-2.7,9.8));
#10573=CARTESIAN_POINT('Origin',(-0.8,-3.2,13.2));
#10574=CARTESIAN_POINT('',(-0.92,-2.9,13.2));
#10575=CARTESIAN_POINT('Origin',(-0.8,-2.9,13.2));
#10576=CARTESIAN_POINT('',(-0.92,-2.7,13.2));
#10577=CARTESIAN_POINT('',(-0.92,-3.2,13.2));
#10578=CARTESIAN_POINT('Origin',(-0.8,-2.7,13.2));
#10579=CARTESIAN_POINT('Origin',(-0.8,-3.2,9.8));
#10580=CARTESIAN_POINT('',(-0.92,-2.9,9.8));
#10581=CARTESIAN_POINT('Origin',(-0.8,-2.9,9.8));
#10582=CARTESIAN_POINT('',(-0.92,-2.7,9.8));
#10583=CARTESIAN_POINT('',(-0.92,-3.2,9.8));
#10584=CARTESIAN_POINT('Origin',(-0.8,-2.7,9.8));
#10585=CARTESIAN_POINT('Origin',(0.8,-3.2,13.2));
#10586=CARTESIAN_POINT('',(0.68,-2.9,13.2));
#10587=CARTESIAN_POINT('Origin',(0.8,-2.9,13.2));
#10588=CARTESIAN_POINT('',(0.68,-2.7,13.2));
#10589=CARTESIAN_POINT('',(0.68,-3.2,13.2));
#10590=CARTESIAN_POINT('Origin',(0.8,-2.7,13.2));
#10591=CARTESIAN_POINT('Origin',(1.,-2.7,9.5));
#10592=CARTESIAN_POINT('',(1.,-2.7,9.5));
#10593=CARTESIAN_POINT('',(-1.,-2.7,9.5));
#10594=CARTESIAN_POINT('',(1.,-2.7,9.5));
#10595=CARTESIAN_POINT('',(-1.,-2.7,13.5));
#10596=CARTESIAN_POINT('',(-1.,-2.7,9.5));
#10597=CARTESIAN_POINT('',(1.,-2.7,13.5));
#10598=CARTESIAN_POINT('',(1.,-2.7,13.5));
#10599=CARTESIAN_POINT('',(1.,-2.7,9.5));
#10600=CARTESIAN_POINT('Origin',(1.,-2.9,9.5));
#10601=CARTESIAN_POINT('',(1.,-2.9,9.5));
#10602=CARTESIAN_POINT('',(1.,-2.9,9.5));
#10603=CARTESIAN_POINT('',(1.,-2.9,13.5));
#10604=CARTESIAN_POINT('',(1.,-2.9,13.5));
#10605=CARTESIAN_POINT('',(1.,-2.9,9.5));
#10606=CARTESIAN_POINT('Origin',(-1.,-2.9,9.5));
#10607=CARTESIAN_POINT('',(-1.,-2.9,9.5));
#10608=CARTESIAN_POINT('',(-1.,-2.9,9.5));
#10609=CARTESIAN_POINT('',(-1.,-2.9,13.5));
#10610=CARTESIAN_POINT('',(-1.,-2.9,13.5));
#10611=CARTESIAN_POINT('',(-1.,-2.9,9.5));
#10612=CARTESIAN_POINT('Origin',(-1.,-2.7,9.5));
#10613=CARTESIAN_POINT('',(-1.,-2.7,9.5));
#10614=CARTESIAN_POINT('',(-1.,-2.7,13.5));
#10615=CARTESIAN_POINT('Origin',(0.,-2.8,13.5));
#10616=CARTESIAN_POINT('Origin',(0.,-2.8,9.5));
#10617=CARTESIAN_POINT('',(0.,0.,0.));
#10618=CARTESIAN_POINT('Origin',(0.8,-3.2,9.8));
#10619=CARTESIAN_POINT('',(0.68,-3.1,9.8));
#10620=CARTESIAN_POINT('Origin',(0.8,-3.1,9.8));
#10621=CARTESIAN_POINT('',(0.68,-2.9,9.8));
#10622=CARTESIAN_POINT('',(0.68,-3.2,9.8));
#10623=CARTESIAN_POINT('Origin',(0.8,-2.9,9.8));
#10624=CARTESIAN_POINT('Origin',(-0.8,-3.2,13.2));
#10625=CARTESIAN_POINT('',(-0.92,-3.1,13.2));
#10626=CARTESIAN_POINT('Origin',(-0.8,-3.1,13.2));
#10627=CARTESIAN_POINT('',(-0.92,-2.9,13.2));
#10628=CARTESIAN_POINT('',(-0.92,-3.2,13.2));
#10629=CARTESIAN_POINT('Origin',(-0.8,-2.9,13.2));
#10630=CARTESIAN_POINT('Origin',(-0.8,-3.2,9.8));
#10631=CARTESIAN_POINT('',(-0.92,-3.1,9.8));
#10632=CARTESIAN_POINT('Origin',(-0.8,-3.1,9.8));
#10633=CARTESIAN_POINT('',(-0.92,-2.9,9.8));
#10634=CARTESIAN_POINT('',(-0.92,-3.2,9.8));
#10635=CARTESIAN_POINT('Origin',(-0.8,-2.9,9.8));
#10636=CARTESIAN_POINT('Origin',(0.8,-3.2,13.2));
#10637=CARTESIAN_POINT('',(0.68,-3.1,13.2));
#10638=CARTESIAN_POINT('Origin',(0.8,-3.1,13.2));
#10639=CARTESIAN_POINT('',(0.68,-2.9,13.2));
#10640=CARTESIAN_POINT('',(0.68,-3.2,13.2));
#10641=CARTESIAN_POINT('Origin',(0.8,-2.9,13.2));
#10642=CARTESIAN_POINT('Origin',(0.6,-3.2,13.));
#10643=CARTESIAN_POINT('',(0.6,-2.9,10.));
#10644=CARTESIAN_POINT('',(0.6,-2.9,13.));
#10645=CARTESIAN_POINT('',(0.6,-2.9,11.25));
#10646=CARTESIAN_POINT('',(0.6,-3.1,10.));
#10647=CARTESIAN_POINT('',(0.6,-3.2,10.));
#10648=CARTESIAN_POINT('',(0.6,-3.1,13.));
#10649=CARTESIAN_POINT('',(0.6,-3.1,11.25));
#10650=CARTESIAN_POINT('',(0.6,-3.2,13.));
#10651=CARTESIAN_POINT('Origin',(-0.6,-3.2,13.));
#10652=CARTESIAN_POINT('',(-0.6,-2.9,13.));
#10653=CARTESIAN_POINT('',(0.2,-2.9,13.));
#10654=CARTESIAN_POINT('',(-0.6,-3.1,13.));
#10655=CARTESIAN_POINT('',(-0.8,-3.1,13.));
#10656=CARTESIAN_POINT('',(-0.6,-3.2,13.));
#10657=CARTESIAN_POINT('Origin',(-0.6,-3.2,10.));
#10658=CARTESIAN_POINT('',(-0.6,-2.9,10.));
#10659=CARTESIAN_POINT('',(-0.6,-2.9,9.75));
#10660=CARTESIAN_POINT('',(-0.6,-3.1,10.));
#10661=CARTESIAN_POINT('',(-0.6,-3.1,9.75));
#10662=CARTESIAN_POINT('',(-0.6,-3.2,10.));
#10663=CARTESIAN_POINT('Origin',(0.6,-3.2,10.));
#10664=CARTESIAN_POINT('',(0.8,-2.9,10.));
#10665=CARTESIAN_POINT('',(-0.2,-3.1,10.));
#10666=CARTESIAN_POINT('Origin',(1.,-2.9,9.5));
#10667=CARTESIAN_POINT('',(1.,-2.9,9.5));
#10668=CARTESIAN_POINT('',(-1.,-2.9,9.5));
#10669=CARTESIAN_POINT('',(1.,-2.9,9.5));
#10670=CARTESIAN_POINT('',(-1.,-2.9,13.5));
#10671=CARTESIAN_POINT('',(-1.,-2.9,9.5));
#10672=CARTESIAN_POINT('',(1.,-2.9,13.5));
#10673=CARTESIAN_POINT('',(1.,-2.9,13.5));
#10674=CARTESIAN_POINT('',(1.,-2.9,9.5));
#10675=CARTESIAN_POINT('Origin',(1.,-3.1,9.5));
#10676=CARTESIAN_POINT('',(1.,-3.1,9.5));
#10677=CARTESIAN_POINT('',(1.,-3.1,9.5));
#10678=CARTESIAN_POINT('',(1.,-3.1,13.5));
#10679=CARTESIAN_POINT('',(1.,-3.1,13.5));
#10680=CARTESIAN_POINT('',(1.,-3.1,9.5));
#10681=CARTESIAN_POINT('Origin',(-1.,-3.1,9.5));
#10682=CARTESIAN_POINT('',(-1.,-3.1,9.5));
#10683=CARTESIAN_POINT('',(-1.,-3.1,9.5));
#10684=CARTESIAN_POINT('',(-1.,-3.1,13.5));
#10685=CARTESIAN_POINT('',(-1.,-3.1,13.5));
#10686=CARTESIAN_POINT('',(-1.,-3.1,9.5));
#10687=CARTESIAN_POINT('Origin',(-1.,-2.9,9.5));
#10688=CARTESIAN_POINT('',(-1.,-2.9,9.5));
#10689=CARTESIAN_POINT('',(-1.,-2.9,13.5));
#10690=CARTESIAN_POINT('Origin',(0.,-3.,13.5));
#10691=CARTESIAN_POINT('Origin',(0.,-3.,9.5));
#10692=CARTESIAN_POINT('',(0.,0.,0.));
#10693=CARTESIAN_POINT('Origin',(-0.83,-3.4,9.6));
#10694=CARTESIAN_POINT('',(-0.83,-3.2,9.62759060350433));
#10695=CARTESIAN_POINT('',(-0.83,-3.3,9.62759060350433));
#10696=CARTESIAN_POINT('',(-0.83,-3.3,9.62759060350433));
#10697=CARTESIAN_POINT('',(-0.83,-3.2,9.97240939649567));
#10698=CARTESIAN_POINT('',(-0.83,-3.2,10.));
#10699=CARTESIAN_POINT('',(-0.83,-3.3,9.97240939649567));
#10700=CARTESIAN_POINT('',(-0.83,-3.3,9.97240939649567));
#10701=CARTESIAN_POINT('',(-0.83,-3.3,9.7));
#10702=CARTESIAN_POINT('Origin',(-0.77,-3.4,10.));
#10703=CARTESIAN_POINT('',(-0.77,-3.3,9.62759060350433));
#10704=CARTESIAN_POINT('',(-0.77,-3.2,9.62759060350433));
#10705=CARTESIAN_POINT('',(-0.77,-3.3,9.62759060350433));
#10706=CARTESIAN_POINT('',(-0.77,-3.3,9.97240939649567));
#10707=CARTESIAN_POINT('',(-0.77,-3.3,9.9));
#10708=CARTESIAN_POINT('',(-0.77,-3.2,9.97240939649567));
#10709=CARTESIAN_POINT('',(-0.77,-3.3,9.97240939649567));
#10710=CARTESIAN_POINT('',(-0.77,-3.2,9.6));
#10711=CARTESIAN_POINT('Origin',(-0.8,-3.2,9.8));
#10712=CARTESIAN_POINT('Origin',(-0.8,-3.2,9.8));
#10713=CARTESIAN_POINT('Origin',(-0.8,-3.2,9.8));
#10714=CARTESIAN_POINT('Origin',(-0.8,-3.3,9.8));
#10715=CARTESIAN_POINT('Origin',(-0.8,-3.3,9.8));
#10716=CARTESIAN_POINT('Origin',(-0.8,-3.3,9.8));
#10717=CARTESIAN_POINT('',(-0.975,-3.3,9.8));
#10718=CARTESIAN_POINT('Origin',(-0.8,-3.3,9.8));
#10719=CARTESIAN_POINT('Origin',(-0.8,-3.3,9.8));
#10720=CARTESIAN_POINT('Origin',(-0.8,-3.1,9.8));
#10721=CARTESIAN_POINT('',(-0.975,-3.1,9.8));
#10722=CARTESIAN_POINT('Origin',(-0.8,-3.1,9.8));
#10723=CARTESIAN_POINT('',(-0.9,-3.1,9.8));
#10724=CARTESIAN_POINT('Origin',(-0.8,-3.1,9.8));
#10725=CARTESIAN_POINT('Origin',(-0.8,-3.3,9.8));
#10726=CARTESIAN_POINT('',(-0.975,-3.3,9.8));
#10727=CARTESIAN_POINT('Origin',(-0.8,-3.1,9.8));
#10728=CARTESIAN_POINT('',(-0.9,-2.1,9.8));
#10729=CARTESIAN_POINT('Origin',(-0.8,-2.1,9.8));
#10730=CARTESIAN_POINT('',(-0.9,-3.1,9.8));
#10731=CARTESIAN_POINT('Origin',(-0.8,-2.1,9.8));
#10732=CARTESIAN_POINT('',(0.,0.,0.));
#10733=CARTESIAN_POINT('Origin',(-0.83,-3.4,13.));
#10734=CARTESIAN_POINT('',(-0.83,-3.2,13.0275906035043));
#10735=CARTESIAN_POINT('',(-0.83,-3.3,13.0275906035043));
#10736=CARTESIAN_POINT('',(-0.83,-3.3,13.0275906035043));
#10737=CARTESIAN_POINT('',(-0.83,-3.2,13.3724093964957));
#10738=CARTESIAN_POINT('',(-0.83,-3.2,13.4));
#10739=CARTESIAN_POINT('',(-0.83,-3.3,13.3724093964957));
#10740=CARTESIAN_POINT('',(-0.83,-3.3,13.3724093964957));
#10741=CARTESIAN_POINT('',(-0.83,-3.3,13.1));
#10742=CARTESIAN_POINT('Origin',(-0.77,-3.4,13.4));
#10743=CARTESIAN_POINT('',(-0.77,-3.3,13.0275906035043));
#10744=CARTESIAN_POINT('',(-0.77,-3.2,13.0275906035043));
#10745=CARTESIAN_POINT('',(-0.77,-3.3,13.0275906035043));
#10746=CARTESIAN_POINT('',(-0.77,-3.3,13.3724093964957));
#10747=CARTESIAN_POINT('',(-0.77,-3.3,13.3));
#10748=CARTESIAN_POINT('',(-0.77,-3.2,13.3724093964957));
#10749=CARTESIAN_POINT('',(-0.77,-3.3,13.3724093964957));
#10750=CARTESIAN_POINT('',(-0.77,-3.2,13.));
#10751=CARTESIAN_POINT('Origin',(-0.8,-3.2,13.2));
#10752=CARTESIAN_POINT('Origin',(-0.8,-3.2,13.2));
#10753=CARTESIAN_POINT('Origin',(-0.8,-3.2,13.2));
#10754=CARTESIAN_POINT('Origin',(-0.8,-3.3,13.2));
#10755=CARTESIAN_POINT('Origin',(-0.8,-3.3,13.2));
#10756=CARTESIAN_POINT('Origin',(-0.8,-3.3,13.2));
#10757=CARTESIAN_POINT('',(-0.975,-3.3,13.2));
#10758=CARTESIAN_POINT('Origin',(-0.8,-3.3,13.2));
#10759=CARTESIAN_POINT('Origin',(-0.8,-3.3,13.2));
#10760=CARTESIAN_POINT('Origin',(-0.8,-3.1,13.2));
#10761=CARTESIAN_POINT('',(-0.975,-3.1,13.2));
#10762=CARTESIAN_POINT('Origin',(-0.8,-3.1,13.2));
#10763=CARTESIAN_POINT('',(-0.9,-3.1,13.2));
#10764=CARTESIAN_POINT('Origin',(-0.8,-3.1,13.2));
#10765=CARTESIAN_POINT('Origin',(-0.8,-3.3,13.2));
#10766=CARTESIAN_POINT('',(-0.975,-3.3,13.2));
#10767=CARTESIAN_POINT('Origin',(-0.8,-3.1,13.2));
#10768=CARTESIAN_POINT('',(-0.9,-2.1,13.2));
#10769=CARTESIAN_POINT('Origin',(-0.8,-2.1,13.2));
#10770=CARTESIAN_POINT('',(-0.9,-3.1,13.2));
#10771=CARTESIAN_POINT('Origin',(-0.8,-2.1,13.2));
#10772=CARTESIAN_POINT('',(0.,0.,0.));
#10773=CARTESIAN_POINT('Origin',(0.77,-3.4,9.6));
#10774=CARTESIAN_POINT('',(0.77,-3.2,9.62759060350433));
#10775=CARTESIAN_POINT('',(0.77,-3.3,9.62759060350433));
#10776=CARTESIAN_POINT('',(0.77,-3.3,9.62759060350433));
#10777=CARTESIAN_POINT('',(0.77,-3.2,9.97240939649567));
#10778=CARTESIAN_POINT('',(0.77,-3.2,10.));
#10779=CARTESIAN_POINT('',(0.77,-3.3,9.97240939649567));
#10780=CARTESIAN_POINT('',(0.77,-3.3,9.97240939649567));
#10781=CARTESIAN_POINT('',(0.77,-3.3,9.7));
#10782=CARTESIAN_POINT('Origin',(0.83,-3.4,10.));
#10783=CARTESIAN_POINT('',(0.83,-3.3,9.62759060350433));
#10784=CARTESIAN_POINT('',(0.83,-3.2,9.62759060350433));
#10785=CARTESIAN_POINT('',(0.83,-3.3,9.62759060350433));
#10786=CARTESIAN_POINT('',(0.83,-3.3,9.97240939649567));
#10787=CARTESIAN_POINT('',(0.83,-3.3,9.9));
#10788=CARTESIAN_POINT('',(0.83,-3.2,9.97240939649567));
#10789=CARTESIAN_POINT('',(0.83,-3.3,9.97240939649567));
#10790=CARTESIAN_POINT('',(0.83,-3.2,9.6));
#10791=CARTESIAN_POINT('Origin',(0.8,-3.2,9.8));
#10792=CARTESIAN_POINT('Origin',(0.8,-3.2,9.8));
#10793=CARTESIAN_POINT('Origin',(0.8,-3.2,9.8));
#10794=CARTESIAN_POINT('Origin',(0.8,-3.3,9.8));
#10795=CARTESIAN_POINT('Origin',(0.8,-3.3,9.8));
#10796=CARTESIAN_POINT('Origin',(0.8,-3.3,9.8));
#10797=CARTESIAN_POINT('',(0.625,-3.3,9.8));
#10798=CARTESIAN_POINT('Origin',(0.8,-3.3,9.8));
#10799=CARTESIAN_POINT('Origin',(0.8,-3.3,9.8));
#10800=CARTESIAN_POINT('Origin',(0.8,-3.1,9.8));
#10801=CARTESIAN_POINT('',(0.625,-3.1,9.8));
#10802=CARTESIAN_POINT('Origin',(0.8,-3.1,9.8));
#10803=CARTESIAN_POINT('',(0.7,-3.1,9.8));
#10804=CARTESIAN_POINT('Origin',(0.8,-3.1,9.8));
#10805=CARTESIAN_POINT('Origin',(0.8,-3.3,9.8));
#10806=CARTESIAN_POINT('',(0.625,-3.3,9.8));
#10807=CARTESIAN_POINT('Origin',(0.8,-3.1,9.8));
#10808=CARTESIAN_POINT('',(0.7,-2.1,9.8));
#10809=CARTESIAN_POINT('Origin',(0.8,-2.1,9.8));
#10810=CARTESIAN_POINT('',(0.7,-3.1,9.8));
#10811=CARTESIAN_POINT('Origin',(0.8,-2.1,9.8));
#10812=CARTESIAN_POINT('',(0.,0.,0.));
#10813=CARTESIAN_POINT('Origin',(0.77,-3.4,13.));
#10814=CARTESIAN_POINT('',(0.77,-3.2,13.0275906035043));
#10815=CARTESIAN_POINT('',(0.77,-3.3,13.0275906035043));
#10816=CARTESIAN_POINT('',(0.77,-3.3,13.0275906035043));
#10817=CARTESIAN_POINT('',(0.77,-3.2,13.3724093964957));
#10818=CARTESIAN_POINT('',(0.77,-3.2,13.4));
#10819=CARTESIAN_POINT('',(0.77,-3.3,13.3724093964957));
#10820=CARTESIAN_POINT('',(0.77,-3.3,13.3724093964957));
#10821=CARTESIAN_POINT('',(0.77,-3.3,13.1));
#10822=CARTESIAN_POINT('Origin',(0.83,-3.4,13.4));
#10823=CARTESIAN_POINT('',(0.83,-3.3,13.0275906035043));
#10824=CARTESIAN_POINT('',(0.83,-3.2,13.0275906035043));
#10825=CARTESIAN_POINT('',(0.83,-3.3,13.0275906035043));
#10826=CARTESIAN_POINT('',(0.83,-3.3,13.3724093964957));
#10827=CARTESIAN_POINT('',(0.83,-3.3,13.3));
#10828=CARTESIAN_POINT('',(0.83,-3.2,13.3724093964957));
#10829=CARTESIAN_POINT('',(0.83,-3.3,13.3724093964957));
#10830=CARTESIAN_POINT('',(0.83,-3.2,13.));
#10831=CARTESIAN_POINT('Origin',(0.8,-3.2,13.2));
#10832=CARTESIAN_POINT('Origin',(0.8,-3.2,13.2));
#10833=CARTESIAN_POINT('Origin',(0.8,-3.2,13.2));
#10834=CARTESIAN_POINT('Origin',(0.8,-3.3,13.2));
#10835=CARTESIAN_POINT('Origin',(0.8,-3.3,13.2));
#10836=CARTESIAN_POINT('Origin',(0.8,-3.3,13.2));
#10837=CARTESIAN_POINT('',(0.625,-3.3,13.2));
#10838=CARTESIAN_POINT('Origin',(0.8,-3.3,13.2));
#10839=CARTESIAN_POINT('Origin',(0.8,-3.3,13.2));
#10840=CARTESIAN_POINT('Origin',(0.8,-3.1,13.2));
#10841=CARTESIAN_POINT('',(0.625,-3.1,13.2));
#10842=CARTESIAN_POINT('Origin',(0.8,-3.1,13.2));
#10843=CARTESIAN_POINT('',(0.7,-3.1,13.2));
#10844=CARTESIAN_POINT('Origin',(0.8,-3.1,13.2));
#10845=CARTESIAN_POINT('Origin',(0.8,-3.3,13.2));
#10846=CARTESIAN_POINT('',(0.625,-3.3,13.2));
#10847=CARTESIAN_POINT('Origin',(0.8,-3.1,13.2));
#10848=CARTESIAN_POINT('',(0.7,-2.1,13.2));
#10849=CARTESIAN_POINT('Origin',(0.8,-2.1,13.2));
#10850=CARTESIAN_POINT('',(0.7,-3.1,13.2));
#10851=CARTESIAN_POINT('Origin',(0.8,-2.1,13.2));
#10852=CARTESIAN_POINT('',(0.,0.,0.));
#10853=CARTESIAN_POINT('Origin',(-2.75,3.36777869765522E-16,14.9));
#10854=CARTESIAN_POINT('',(-2.975,3.09223316784707E-16,15.));
#10855=CARTESIAN_POINT('Origin',(-2.75,3.36777869765522E-16,15.));
#10856=CARTESIAN_POINT('',(-2.975,3.64332422746338E-16,15.1));
#10857=CARTESIAN_POINT('',(-2.975,3.09223316784707E-16,14.9));
#10858=CARTESIAN_POINT('Origin',(-2.75,3.36777869765522E-16,15.1));
#10859=CARTESIAN_POINT('Origin',(1.68388934882761E-16,2.75,14.9));
#10860=CARTESIAN_POINT('',(-0.225,2.75,15.));
#10861=CARTESIAN_POINT('Origin',(1.68388934882761E-16,2.75,15.));
#10862=CARTESIAN_POINT('',(-0.225,2.75,15.1));
#10863=CARTESIAN_POINT('',(-0.225,2.75,14.9));
#10864=CARTESIAN_POINT('Origin',(1.68388934882761E-16,2.75,15.1));
#10865=CARTESIAN_POINT('Origin',(2.75,0.,14.9));
#10866=CARTESIAN_POINT('',(2.525,-2.75545529808155E-17,15.));
#10867=CARTESIAN_POINT('Origin',(2.75,0.,15.));
#10868=CARTESIAN_POINT('',(2.525,2.75545529808155E-17,15.1));
#10869=CARTESIAN_POINT('',(2.525,-2.75545529808155E-17,14.9));
#10870=CARTESIAN_POINT('Origin',(2.75,0.,15.1));
#10871=CARTESIAN_POINT('Origin',(-5.05166804648283E-16,-2.75,14.9));
#10872=CARTESIAN_POINT('',(-0.225000000000001,-2.75,15.));
#10873=CARTESIAN_POINT('Origin',(-5.05166804648283E-16,-2.75,15.));
#10874=CARTESIAN_POINT('',(-0.225000000000001,-2.75,15.1));
#10875=CARTESIAN_POINT('',(-0.225000000000001,-2.75,14.9));
#10876=CARTESIAN_POINT('Origin',(-5.05166804648283E-16,-2.75,15.1));
#10877=CARTESIAN_POINT('Origin',(0.,0.,15.));
#10878=CARTESIAN_POINT('',(-2.5,-3.06161699786838E-16,15.1));
#10879=CARTESIAN_POINT('Origin',(0.,0.,15.1));
#10880=CARTESIAN_POINT('',(-2.5,-3.06161699786838E-16,15.));
#10881=CARTESIAN_POINT('',(-2.5,-3.06161699786838E-16,15.));
#10882=CARTESIAN_POINT('Origin',(0.,0.,15.));
#10883=CARTESIAN_POINT('Origin',(0.,0.,15.));
#10884=CARTESIAN_POINT('',(-3.,-3.67394039744206E-16,15.1));
#10885=CARTESIAN_POINT('Origin',(0.,0.,15.1));
#10886=CARTESIAN_POINT('',(-3.,-3.67394039744206E-16,15.));
#10887=CARTESIAN_POINT('',(-3.,-3.67394039744206E-16,15.));
#10888=CARTESIAN_POINT('Origin',(0.,0.,15.));
#10889=CARTESIAN_POINT('Origin',(0.,0.,15.1));
#10890=CARTESIAN_POINT('Origin',(0.,0.,15.));
#10891=CARTESIAN_POINT('',(0.,0.,0.));
#10892=CARTESIAN_POINT('Origin',(0.,0.,15.));
#10893=CARTESIAN_POINT('',(-0.6,-7.34788079488412E-17,15.1));
#10894=CARTESIAN_POINT('Origin',(0.,0.,15.1));
#10895=CARTESIAN_POINT('',(-0.6,7.34788079488412E-17,15.7));
#10896=CARTESIAN_POINT('',(-0.6,-7.34788079488412E-17,15.));
#10897=CARTESIAN_POINT('Origin',(0.,0.,15.7));
#10898=CARTESIAN_POINT('Origin',(-2.75,3.36777869765522E-16,14.9));
#10899=CARTESIAN_POINT('',(-2.975,3.09223316784707E-16,15.1));
#10900=CARTESIAN_POINT('Origin',(-2.75,3.36777869765522E-16,15.1));
#10901=CARTESIAN_POINT('',(-2.975,3.64332422746338E-16,15.7));
#10902=CARTESIAN_POINT('',(-2.975,3.09223316784707E-16,14.9));
#10903=CARTESIAN_POINT('Origin',(-2.75,3.36777869765522E-16,15.7));
#10904=CARTESIAN_POINT('Origin',(1.68388934882761E-16,2.75,14.9));
#10905=CARTESIAN_POINT('',(-0.225,2.75,15.1));
#10906=CARTESIAN_POINT('Origin',(1.68388934882761E-16,2.75,15.1));
#10907=CARTESIAN_POINT('',(-0.225,2.75,15.7));
#10908=CARTESIAN_POINT('',(-0.225,2.75,14.9));
#10909=CARTESIAN_POINT('Origin',(1.68388934882761E-16,2.75,15.7));
#10910=CARTESIAN_POINT('Origin',(2.75,0.,14.9));
#10911=CARTESIAN_POINT('',(2.525,-2.75545529808155E-17,15.1));
#10912=CARTESIAN_POINT('Origin',(2.75,0.,15.1));
#10913=CARTESIAN_POINT('',(2.525,2.75545529808155E-17,15.7));
#10914=CARTESIAN_POINT('',(2.525,-2.75545529808155E-17,14.9));
#10915=CARTESIAN_POINT('Origin',(2.75,0.,15.7));
#10916=CARTESIAN_POINT('Origin',(-5.05166804648283E-16,-2.75,14.9));
#10917=CARTESIAN_POINT('',(-0.225000000000001,-2.75,15.1));
#10918=CARTESIAN_POINT('Origin',(-5.05166804648283E-16,-2.75,15.1));
#10919=CARTESIAN_POINT('',(-0.225000000000001,-2.75,15.7));
#10920=CARTESIAN_POINT('',(-0.225000000000001,-2.75,14.9));
#10921=CARTESIAN_POINT('Origin',(-5.05166804648283E-16,-2.75,15.7));
#10922=CARTESIAN_POINT('Origin',(0.,0.,15.1));
#10923=CARTESIAN_POINT('',(-3.,-3.67394039744206E-16,15.7));
#10924=CARTESIAN_POINT('Origin',(0.,0.,15.7));
#10925=CARTESIAN_POINT('',(-3.,-3.67394039744206E-16,15.1));
#10926=CARTESIAN_POINT('',(-3.,-3.67394039744206E-16,15.1));
#10927=CARTESIAN_POINT('Origin',(0.,0.,15.1));
#10928=CARTESIAN_POINT('Origin',(0.,0.,15.7));
#10929=CARTESIAN_POINT('Origin',(0.,0.,15.1));
#10930=CARTESIAN_POINT('',(0.,0.,0.));
#10931=CARTESIAN_POINT('Origin',(0.,0.,15.1));
#10932=CARTESIAN_POINT('',(-0.075,-9.18485099360515E-18,15.2));
#10933=CARTESIAN_POINT('Origin',(0.,0.,15.2));
#10934=CARTESIAN_POINT('',(-0.075,9.18485099360515E-18,16.2));
#10935=CARTESIAN_POINT('',(-0.075,-9.18485099360515E-18,15.1));
#10936=CARTESIAN_POINT('Origin',(0.,0.,16.2));
#10937=CARTESIAN_POINT('Origin',(0.,0.,15.7));
#10938=CARTESIAN_POINT('',(-1.,-1.22464679914735E-16,15.7));
#10939=CARTESIAN_POINT('Origin',(0.,0.,15.7));
#10940=CARTESIAN_POINT('',(-0.6,-7.34788079488412E-17,15.7));
#10941=CARTESIAN_POINT('Origin',(0.,0.,15.7));
#10942=CARTESIAN_POINT('Origin',(0.,0.,15.7));
#10943=CARTESIAN_POINT('',(-1.,-1.22464679914735E-16,16.2));
#10944=CARTESIAN_POINT('Origin',(0.,0.,16.2));
#10945=CARTESIAN_POINT('',(-1.,-1.22464679914735E-16,15.7));
#10946=CARTESIAN_POINT('Origin',(0.,0.,16.2));
#10947=CARTESIAN_POINT('Origin',(0.,0.,15.2));
#10948=CARTESIAN_POINT('',(-0.6,-7.34788079488412E-17,15.2));
#10949=CARTESIAN_POINT('',(-0.6,-7.34788079488412E-17,15.2));
#10950=CARTESIAN_POINT('Origin',(0.,0.,15.2));
#10951=CARTESIAN_POINT('Origin',(0.,0.,15.2));
#10952=CARTESIAN_POINT('',(0.,0.,0.));
#10953=CARTESIAN_POINT('Origin',(-5.,3.5,-0.4));
#10954=CARTESIAN_POINT('',(-5.,3.5,-0.4));
#10955=CARTESIAN_POINT('',(-7.,3.5,-0.4));
#10956=CARTESIAN_POINT('',(-5.,3.5,-0.4));
#10957=CARTESIAN_POINT('',(-7.,3.5,0.));
#10958=CARTESIAN_POINT('',(-7.,3.5,-0.4));
#10959=CARTESIAN_POINT('',(-5.,3.5,0.));
#10960=CARTESIAN_POINT('',(-5.,3.5,0.));
#10961=CARTESIAN_POINT('',(-5.,3.5,-0.4));
#10962=CARTESIAN_POINT('Origin',(-5.,-3.5,-0.4));
#10963=CARTESIAN_POINT('',(-5.,-3.5,-0.4));
#10964=CARTESIAN_POINT('',(-5.,-3.5,-0.4));
#10965=CARTESIAN_POINT('',(-5.,-3.5,0.));
#10966=CARTESIAN_POINT('',(-5.,-3.5,0.));
#10967=CARTESIAN_POINT('',(-5.,-3.5,-0.4));
#10968=CARTESIAN_POINT('Origin',(-7.,-3.5,-0.4));
#10969=CARTESIAN_POINT('',(-7.,-3.5,-0.4));
#10970=CARTESIAN_POINT('',(-7.,-3.5,-0.4));
#10971=CARTESIAN_POINT('',(-7.,-3.5,0.));
#10972=CARTESIAN_POINT('',(-7.,-3.5,0.));
#10973=CARTESIAN_POINT('',(-7.,-3.5,-0.4));
#10974=CARTESIAN_POINT('Origin',(-7.,3.5,-0.4));
#10975=CARTESIAN_POINT('',(-7.,3.5,-0.4));
#10976=CARTESIAN_POINT('',(-7.,3.5,0.));
#10977=CARTESIAN_POINT('Origin',(-6.,0.,0.));
#10978=CARTESIAN_POINT('Origin',(-6.,0.,-0.4));
#10979=CARTESIAN_POINT('',(0.,0.,0.));
#10980=CARTESIAN_POINT('Origin',(7.,3.5,-0.4));
#10981=CARTESIAN_POINT('',(7.,3.5,-0.4));
#10982=CARTESIAN_POINT('',(5.,3.5,-0.4));
#10983=CARTESIAN_POINT('',(7.,3.5,-0.4));
#10984=CARTESIAN_POINT('',(5.,3.5,0.));
#10985=CARTESIAN_POINT('',(5.,3.5,-0.4));
#10986=CARTESIAN_POINT('',(7.,3.5,0.));
#10987=CARTESIAN_POINT('',(7.,3.5,0.));
#10988=CARTESIAN_POINT('',(7.,3.5,-0.4));
#10989=CARTESIAN_POINT('Origin',(7.,-3.5,-0.4));
#10990=CARTESIAN_POINT('',(7.,-3.5,-0.4));
#10991=CARTESIAN_POINT('',(7.,-3.5,-0.4));
#10992=CARTESIAN_POINT('',(7.,-3.5,0.));
#10993=CARTESIAN_POINT('',(7.,-3.5,0.));
#10994=CARTESIAN_POINT('',(7.,-3.5,-0.4));
#10995=CARTESIAN_POINT('Origin',(5.,-3.5,-0.4));
#10996=CARTESIAN_POINT('',(5.,-3.5,-0.4));
#10997=CARTESIAN_POINT('',(5.,-3.5,-0.4));
#10998=CARTESIAN_POINT('',(5.,-3.5,0.));
#10999=CARTESIAN_POINT('',(5.,-3.5,0.));
#11000=CARTESIAN_POINT('',(5.,-3.5,-0.4));
#11001=CARTESIAN_POINT('Origin',(5.,3.5,-0.4));
#11002=CARTESIAN_POINT('',(5.,3.5,-0.4));
#11003=CARTESIAN_POINT('',(5.,3.5,0.));
#11004=CARTESIAN_POINT('Origin',(6.,0.,0.));
#11005=CARTESIAN_POINT('Origin',(6.,0.,-0.4));
#11006=CARTESIAN_POINT('',(0.,0.,0.));
#11007=CARTESIAN_POINT('Origin',(0.115470053837925,-0.5,-0.2));
#11008=CARTESIAN_POINT('',(0.23094010767585,-0.5,0.));
#11009=CARTESIAN_POINT('',(0.115470053837925,-0.5,-0.2));
#11010=CARTESIAN_POINT('',(0.23094010767585,-0.5,0.));
#11011=CARTESIAN_POINT('',(0.115470053837925,-0.8,-0.2));
#11012=CARTESIAN_POINT('',(0.115470053837925,-0.5,-0.2));
#11013=CARTESIAN_POINT('',(0.23094010767585,-0.8,0.));
#11014=CARTESIAN_POINT('',(0.23094010767585,-0.8,0.));
#11015=CARTESIAN_POINT('',(0.23094010767585,-0.5,0.));
#11016=CARTESIAN_POINT('Origin',(-0.115470053837925,-0.5,-0.2));
#11017=CARTESIAN_POINT('',(-0.115470053837925,-0.5,-0.2));
#11018=CARTESIAN_POINT('',(0.115470053837925,-0.5,-0.2));
#11019=CARTESIAN_POINT('',(-0.115470053837925,-0.8,-0.2));
#11020=CARTESIAN_POINT('',(-0.115470053837925,-0.5,-0.2));
#11021=CARTESIAN_POINT('',(0.115470053837925,-0.8,-0.2));
#11022=CARTESIAN_POINT('Origin',(-0.23094010767585,-0.5,-2.77555756156289E-17));
#11023=CARTESIAN_POINT('',(-0.23094010767585,-0.5,-2.82820063659975E-17));
#11024=CARTESIAN_POINT('',(-0.115470053837925,-0.5,-0.2));
#11025=CARTESIAN_POINT('',(-0.23094010767585,-0.8,-2.77555756156289E-17));
#11026=CARTESIAN_POINT('',(-0.23094010767585,-0.5,-2.82820063659975E-17));
#11027=CARTESIAN_POINT('',(-0.115470053837925,-0.8,-0.2));
#11028=CARTESIAN_POINT('Origin',(-0.115470053837925,-0.5,0.2));
#11029=CARTESIAN_POINT('',(-0.115470053837925,-0.5,0.2));
#11030=CARTESIAN_POINT('',(-0.23094010767585,-0.5,-2.82820063659975E-17));
#11031=CARTESIAN_POINT('',(-0.115470053837925,-0.8,0.2));
#11032=CARTESIAN_POINT('',(-0.115470053837925,-0.5,0.2));
#11033=CARTESIAN_POINT('',(-0.23094010767585,-0.8,-2.82820063659975E-17));
#11034=CARTESIAN_POINT('Origin',(0.115470053837925,-0.5,0.2));
#11035=CARTESIAN_POINT('',(0.115470053837925,-0.5,0.2));
#11036=CARTESIAN_POINT('',(-0.115470053837925,-0.5,0.2));
#11037=CARTESIAN_POINT('',(0.115470053837925,-0.8,0.2));
#11038=CARTESIAN_POINT('',(0.115470053837925,-0.5,0.2));
#11039=CARTESIAN_POINT('',(-0.115470053837925,-0.8,0.2));
#11040=CARTESIAN_POINT('Origin',(0.23094010767585,-0.5,0.));
#11041=CARTESIAN_POINT('',(0.115470053837925,-0.5,0.2));
#11042=CARTESIAN_POINT('',(0.115470053837925,-0.8,0.2));
#11043=CARTESIAN_POINT('Origin',(0.,-0.5,0.));
#11044=CARTESIAN_POINT('Origin',(0.,-0.8,0.));
#11045=CARTESIAN_POINT('Origin',(0.,-1.4,0.));
#11046=CARTESIAN_POINT('',(-0.24505,-1.4,3.00099698131059E-17));
#11047=CARTESIAN_POINT('Origin',(0.,-1.4,0.));
#11048=CARTESIAN_POINT('Origin',(0.375,0.5,0.));
#11049=CARTESIAN_POINT('',(-0.375,0.5,-4.59242549680257E-17));
#11050=CARTESIAN_POINT('Origin',(0.,0.5,0.));
#11051=CARTESIAN_POINT('Origin',(0.,0.475,0.));
#11052=CARTESIAN_POINT('',(-0.425,0.45,-5.20474889637625E-17));
#11053=CARTESIAN_POINT('Origin',(0.,0.45,0.));
#11054=CARTESIAN_POINT('',(-0.4,0.475,-4.89858719658941E-17));
#11055=CARTESIAN_POINT('Origin',(0.,0.24,0.));
#11056=CARTESIAN_POINT('',(-0.425,0.0299999999999998,-5.20474889637625E-17));
#11057=CARTESIAN_POINT('Origin',(0.,0.0299999999999998,0.));
#11058=CARTESIAN_POINT('',(-0.425,0.24,-5.20474889637625E-17));
#11059=CARTESIAN_POINT('Origin',(0.,0.0150000000000001,0.));
#11060=CARTESIAN_POINT('',(-0.395,4.85722573273506E-17,-4.83735485663204E-17));
#11061=CARTESIAN_POINT('Origin',(0.,0.,0.));
#11062=CARTESIAN_POINT('',(-0.41,0.0150000000000001,-5.02105187650415E-17));
#11063=CARTESIAN_POINT('Origin',(0.27,0.,0.));
#11064=CARTESIAN_POINT('',(-0.27,0.,-3.30654635769785E-17));
#11065=CARTESIAN_POINT('Origin',(0.,0.,0.));
#11066=CARTESIAN_POINT('Origin',(0.,-0.02,0.));
#11067=CARTESIAN_POINT('',(-0.24505,-0.0498999999999999,3.00099698131059E-17));
#11068=CARTESIAN_POINT('Origin',(0.,-0.0498999999999999,0.));
#11069=CARTESIAN_POINT('',(-0.26,-0.02,-3.18408167778312E-17));
#11070=CARTESIAN_POINT('Origin',(0.,-0.995,0.));
#11071=CARTESIAN_POINT('',(-0.24505,-0.995,-3.00099698131059E-17));
#11072=CARTESIAN_POINT('',(0.,0.,0.));
#11073=CARTESIAN_POINT('',(0.,0.,0.));
#11074=CARTESIAN_POINT('Origin',(0.,0.6,0.));
#11075=CARTESIAN_POINT('',(-0.43,0.6,5.26598123633362E-17));
#11076=CARTESIAN_POINT('Origin',(0.,0.6,0.));
#11077=CARTESIAN_POINT('',(-0.43,0.7,-5.26598123633362E-17));
#11078=CARTESIAN_POINT('',(-0.43,0.6,5.26598123633362E-17));
#11079=CARTESIAN_POINT('Origin',(0.,0.7,0.));
#11080=CARTESIAN_POINT('Origin',(0.,0.6,0.));
#11081=CARTESIAN_POINT('',(-0.2,0.6,2.44929359829471E-17));
#11082=CARTESIAN_POINT('Origin',(0.,0.6,0.));
#11083=CARTESIAN_POINT('Origin',(0.,0.5,-1.11022302462516E-16));
#11084=CARTESIAN_POINT('',(0.346410161513776,0.5,0.6));
#11085=CARTESIAN_POINT('',(0.692820323027551,0.5,0.));
#11086=CARTESIAN_POINT('',(0.346410161513776,0.5,0.6));
#11087=CARTESIAN_POINT('',(0.346410161513776,0.5,-0.6));
#11088=CARTESIAN_POINT('',(0.692820323027551,0.5,0.));
#11089=CARTESIAN_POINT('',(-0.346410161513775,0.5,-0.6));
#11090=CARTESIAN_POINT('',(0.346410161513776,0.5,-0.6));
#11091=CARTESIAN_POINT('',(-0.692820323027551,0.5,-8.48460190979926E-17));
#11092=CARTESIAN_POINT('',(-0.346410161513775,0.5,-0.6));
#11093=CARTESIAN_POINT('',(-0.346410161513776,0.5,0.6));
#11094=CARTESIAN_POINT('',(-0.692820323027551,0.5,-8.48460190979926E-17));
#11095=CARTESIAN_POINT('',(-0.346410161513776,0.5,0.6));
#11096=CARTESIAN_POINT('',(-0.525,0.5,-6.4293956955236E-17));
#11097=CARTESIAN_POINT('Origin',(0.,0.5,0.));
#11098=CARTESIAN_POINT('Origin',(0.,0.,-1.11022302462516E-16));
#11099=CARTESIAN_POINT('',(0.346410161513776,0.,0.6));
#11100=CARTESIAN_POINT('',(0.692820323027551,0.,0.));
#11101=CARTESIAN_POINT('',(0.346410161513776,0.,0.6));
#11102=CARTESIAN_POINT('',(-0.346410161513776,0.,0.6));
#11103=CARTESIAN_POINT('',(-0.346410161513776,0.,0.6));
#11104=CARTESIAN_POINT('',(-0.692820323027551,0.,-8.48460190979926E-17));
#11105=CARTESIAN_POINT('',(-0.692820323027551,0.,-8.48460190979926E-17));
#11106=CARTESIAN_POINT('',(-0.346410161513775,0.,-0.6));
#11107=CARTESIAN_POINT('',(-0.346410161513775,0.,-0.6));
#11108=CARTESIAN_POINT('',(0.346410161513776,0.,-0.6));
#11109=CARTESIAN_POINT('',(0.346410161513776,0.,-0.6));
#11110=CARTESIAN_POINT('',(0.692820323027551,0.,0.));
#11111=CARTESIAN_POINT('',(-0.515,0.,-6.30693101560887E-17));
#11112=CARTESIAN_POINT('Origin',(0.,0.,0.));
#11113=CARTESIAN_POINT('Origin',(-0.346410161513776,0.,0.6));
#11114=CARTESIAN_POINT('',(0.346410161513776,0.,0.6));
#11115=CARTESIAN_POINT('',(-0.346410161513776,0.,0.6));
#11116=CARTESIAN_POINT('Origin',(-0.692820323027551,0.,-8.48460190979926E-17));
#11117=CARTESIAN_POINT('',(-0.692820323027551,0.,-8.48460190979926E-17));
#11118=CARTESIAN_POINT('Origin',(-0.346410161513775,0.,-0.6));
#11119=CARTESIAN_POINT('',(-0.346410161513775,0.,-0.6));
#11120=CARTESIAN_POINT('Origin',(0.346410161513776,0.,-0.6));
#11121=CARTESIAN_POINT('',(0.346410161513776,0.,-0.6));
#11122=CARTESIAN_POINT('Origin',(0.692820323027551,0.,0.));
#11123=CARTESIAN_POINT('',(0.692820323027551,0.,0.));
#11124=CARTESIAN_POINT('Origin',(0.346410161513776,0.,0.6));
#11125=CARTESIAN_POINT('Origin',(0.46,0.7,0.));
#11126=CARTESIAN_POINT('',(-0.46,0.7,-5.63337527607782E-17));
#11127=CARTESIAN_POINT('Origin',(0.,0.7,0.));
#11128=CARTESIAN_POINT('Origin',(0.,1.2,0.));
#11129=CARTESIAN_POINT('',(-0.46,1.7,-5.63337527607782E-17));
#11130=CARTESIAN_POINT('',(-0.46,1.2,-5.63337527607782E-17));
#11131=CARTESIAN_POINT('Origin',(0.,1.7,0.));
#11132=CARTESIAN_POINT('Origin',(0.525,1.7,0.));
#11133=CARTESIAN_POINT('',(-0.525,1.7,-6.4293956955236E-17));
#11134=CARTESIAN_POINT('Origin',(0.,1.7,0.));
#11135=CARTESIAN_POINT('Origin',(0.,1.1,0.));
#11136=CARTESIAN_POINT('',(-0.525,1.1,-6.4293956955236E-17));
#11137=CARTESIAN_POINT('Origin',(0.,-0.325,0.));
#11138=CARTESIAN_POINT('',(-0.515,-0.65,-6.30693101560887E-17));
#11139=CARTESIAN_POINT('Origin',(0.,-0.65,0.));
#11140=CARTESIAN_POINT('',(-0.515,-0.325,-6.30693101560887E-17));
#11141=CARTESIAN_POINT('Origin',(0.2,-0.65,0.));
#11142=CARTESIAN_POINT('',(-0.2,-0.65,-2.44929359829471E-17));
#11143=CARTESIAN_POINT('Origin',(0.,-0.65,0.));
#11144=CARTESIAN_POINT('Origin',(0.,0.0249999999999999,0.));
#11145=CARTESIAN_POINT('',(-0.2,0.0249999999999999,-2.44929359829471E-17));
#11146=CARTESIAN_POINT('',(0.,0.,0.));
#11147=CARTESIAN_POINT('Origin',(0.475,1.95,0.));
#11148=CARTESIAN_POINT('',(-0.475,1.95,-5.81707229594993E-17));
#11149=CARTESIAN_POINT('Origin',(0.,1.95,0.));
#11150=CARTESIAN_POINT('',(-0.31,1.95,-3.7964050773568E-17));
#11151=CARTESIAN_POINT('Origin',(0.,1.95,0.));
#11152=CARTESIAN_POINT('Origin',(0.,1.825,0.));
#11153=CARTESIAN_POINT('',(-0.475,1.7,-5.81707229594993E-17));
#11154=CARTESIAN_POINT('Origin',(0.,1.7,0.));
#11155=CARTESIAN_POINT('',(-0.475,1.825,-5.81707229594993E-17));
#11156=CARTESIAN_POINT('Origin',(0.355,1.7,0.));
#11157=CARTESIAN_POINT('',(-0.355,1.7,-4.3474961369731E-17));
#11158=CARTESIAN_POINT('Origin',(0.,1.7,0.));
#11159=CARTESIAN_POINT('Origin',(0.,1.55,0.));
#11160=CARTESIAN_POINT('',(-0.355,1.4,-4.3474961369731E-17));
#11161=CARTESIAN_POINT('Origin',(0.,1.4,0.));
#11162=CARTESIAN_POINT('',(-0.355,1.55,-4.3474961369731E-17));
#11163=CARTESIAN_POINT('Origin',(0.31,1.4,0.));
#11164=CARTESIAN_POINT('',(-0.31,1.4,-3.7964050773568E-17));
#11165=CARTESIAN_POINT('Origin',(0.,1.4,0.));
#11166=CARTESIAN_POINT('Origin',(0.,1.675,0.));
#11167=CARTESIAN_POINT('',(-0.31,1.675,-3.7964050773568E-17));
#11168=CARTESIAN_POINT('',(0.,0.,0.));
#11169=CARTESIAN_POINT('',(0.,0.,0.));
#11170=CARTESIAN_POINT('',(0.,0.,0.));
#11171=CARTESIAN_POINT('Origin',(0.,-0.4,0.));
#11172=CARTESIAN_POINT('',(1.01036297108185,-0.4,0.));
#11173=CARTESIAN_POINT('',(0.505181485540923,-0.4,0.875));
#11174=CARTESIAN_POINT('',(0.505181485540923,-0.4,0.875));
#11175=CARTESIAN_POINT('',(-0.505181485540923,-0.4,0.875));
#11176=CARTESIAN_POINT('',(-0.505181485540923,-0.4,0.875));
#11177=CARTESIAN_POINT('',(-1.01036297108185,-0.4,-1.23733777851239E-16));
#11178=CARTESIAN_POINT('',(-1.01036297108185,-0.4,-1.23733777851239E-16));
#11179=CARTESIAN_POINT('',(-0.505181485540922,-0.4,-0.875));
#11180=CARTESIAN_POINT('',(-0.505181485540922,-0.4,-0.875));
#11181=CARTESIAN_POINT('',(0.505181485540923,-0.4,-0.875));
#11182=CARTESIAN_POINT('',(0.505181485540923,-0.4,-0.875));
#11183=CARTESIAN_POINT('',(1.01036297108185,-0.4,0.));
#11184=CARTESIAN_POINT('',(-0.685,-0.4,-8.38883057415937E-17));
#11185=CARTESIAN_POINT('Origin',(0.,-0.4,0.));
#11186=CARTESIAN_POINT('Origin',(0.,0.4,0.));
#11187=CARTESIAN_POINT('',(0.505181485540923,0.4,0.875));
#11188=CARTESIAN_POINT('',(1.01036297108185,0.4,0.));
#11189=CARTESIAN_POINT('',(0.505181485540923,0.4,0.875));
#11190=CARTESIAN_POINT('',(0.505181485540923,0.4,-0.875));
#11191=CARTESIAN_POINT('',(1.01036297108185,0.4,0.));
#11192=CARTESIAN_POINT('',(-0.505181485540922,0.4,-0.875));
#11193=CARTESIAN_POINT('',(0.505181485540923,0.4,-0.875));
#11194=CARTESIAN_POINT('',(-1.01036297108185,0.4,-1.23733777851239E-16));
#11195=CARTESIAN_POINT('',(-0.505181485540922,0.4,-0.875));
#11196=CARTESIAN_POINT('',(-0.505181485540923,0.4,0.875));
#11197=CARTESIAN_POINT('',(-1.01036297108185,0.4,-1.23733777851239E-16));
#11198=CARTESIAN_POINT('',(-0.505181485540923,0.4,0.875));
#11199=CARTESIAN_POINT('',(-0.685,0.4,8.38883057415937E-17));
#11200=CARTESIAN_POINT('Origin',(0.,0.4,0.));
#11201=CARTESIAN_POINT('Origin',(-0.505181485540923,0.,0.875));
#11202=CARTESIAN_POINT('',(0.505181485540923,0.,0.875));
#11203=CARTESIAN_POINT('',(-0.505181485540923,0.,0.875));
#11204=CARTESIAN_POINT('Origin',(-1.01036297108185,0.,-1.23733777851239E-16));
#11205=CARTESIAN_POINT('',(-1.01036297108185,0.,-1.23733777851239E-16));
#11206=CARTESIAN_POINT('Origin',(-0.505181485540922,0.,-0.875));
#11207=CARTESIAN_POINT('',(-0.505181485540922,0.,-0.875));
#11208=CARTESIAN_POINT('Origin',(0.505181485540923,0.,-0.875));
#11209=CARTESIAN_POINT('',(0.505181485540923,0.,-0.875));
#11210=CARTESIAN_POINT('Origin',(1.01036297108185,0.,0.));
#11211=CARTESIAN_POINT('',(1.01036297108185,0.,0.));
#11212=CARTESIAN_POINT('Origin',(0.505181485540923,0.,0.875));
#11213=CARTESIAN_POINT('Origin',(0.,0.,0.));
#11214=CARTESIAN_POINT('',(-0.685,1.82,-8.38883057415937E-17));
#11215=CARTESIAN_POINT('',(-0.685,0.,-8.38883057415937E-17));
#11216=CARTESIAN_POINT('Origin',(0.,1.82,0.));
#11217=CARTESIAN_POINT('Origin',(0.605,1.9,0.));
#11218=CARTESIAN_POINT('',(-0.605,1.9,-7.40911313484149E-17));
#11219=CARTESIAN_POINT('Origin',(0.,1.9,0.));
#11220=CARTESIAN_POINT('',(-0.46,1.9,-5.63337527607782E-17));
#11221=CARTESIAN_POINT('Origin',(0.,1.9,0.));
#11222=CARTESIAN_POINT('Origin',(0.,1.86,0.));
#11223=CARTESIAN_POINT('',(-0.645,1.86,-7.89897185450043E-17));
#11224=CARTESIAN_POINT('Origin',(0.,0.,0.));
#11225=CARTESIAN_POINT('',(-0.685,-1.82,-8.38883057415937E-17));
#11226=CARTESIAN_POINT('Origin',(0.,-1.82,0.));
#11227=CARTESIAN_POINT('',(-0.685,0.,-8.38883057415937E-17));
#11228=CARTESIAN_POINT('Origin',(0.,-1.86,0.));
#11229=CARTESIAN_POINT('',(-0.605,-1.9,-7.40911313484149E-17));
#11230=CARTESIAN_POINT('Origin',(0.,-1.9,0.));
#11231=CARTESIAN_POINT('',(-0.645,-1.86,-7.89897185450043E-17));
#11232=CARTESIAN_POINT('Origin',(0.46,-1.9,0.));
#11233=CARTESIAN_POINT('',(-0.46,-1.9,-5.63337527607782E-17));
#11234=CARTESIAN_POINT('Origin',(0.,-1.9,0.));
#11235=CARTESIAN_POINT('Origin',(0.,0.,0.));
#11236=CARTESIAN_POINT('',(-0.46,0.,-5.63337527607782E-17));
#11237=CARTESIAN_POINT('',(0.,0.,0.));
#11238=CARTESIAN_POINT('Origin',(0.3,0.4,0.));
#11239=CARTESIAN_POINT('',(-0.3,0.4,-3.67394039744206E-17));
#11240=CARTESIAN_POINT('Origin',(0.,0.4,0.));
#11241=CARTESIAN_POINT('Origin',(0.,0.375,0.));
#11242=CARTESIAN_POINT('',(-0.35,0.35,-4.28626379701573E-17));
#11243=CARTESIAN_POINT('Origin',(0.,0.35,0.));
#11244=CARTESIAN_POINT('',(-0.325,0.375,-3.9801020972289E-17));
#11245=CARTESIAN_POINT('Origin',(0.,0.19,0.));
#11246=CARTESIAN_POINT('',(-0.35,0.03,-4.28626379701574E-17));
#11247=CARTESIAN_POINT('Origin',(0.,0.03,0.));
#11248=CARTESIAN_POINT('',(-0.35,0.19,-4.28626379701574E-17));
#11249=CARTESIAN_POINT('Origin',(0.,0.0149999999999999,0.));
#11250=CARTESIAN_POINT('',(-0.32,-3.29597460435593E-17,-3.91886975727153E-17));
#11251=CARTESIAN_POINT('Origin',(0.,0.,0.));
#11252=CARTESIAN_POINT('',(-0.335,0.0149999999999999,-4.10256677714363E-17));
#11253=CARTESIAN_POINT('Origin',(0.22,0.,0.));
#11254=CARTESIAN_POINT('',(-0.22,-6.93889390390723E-18,-2.69422295812418E-17));
#11255=CARTESIAN_POINT('Origin',(0.,0.,0.));
#11256=CARTESIAN_POINT('Origin',(0.,-0.02,0.));
#11257=CARTESIAN_POINT('',(-0.1954,-0.0492,2.39295984553393E-17));
#11258=CARTESIAN_POINT('Origin',(0.,-0.0492,0.));
#11259=CARTESIAN_POINT('',(-0.21,-0.02,-2.57175827820944E-17));
#11260=CARTESIAN_POINT('Origin',(0.,-0.8,0.));
#11261=CARTESIAN_POINT('',(-0.1954,-1.5646,2.39295984553393E-17));
#11262=CARTESIAN_POINT('Origin',(0.,-1.5646,0.));
#11263=CARTESIAN_POINT('',(-0.1954,-0.8,-2.39295984553393E-17));
#11264=CARTESIAN_POINT('Origin',(0.,-1.58,0.));
#11265=CARTESIAN_POINT('',(-0.16,-1.6,-1.95943487863577E-17));
#11266=CARTESIAN_POINT('Origin',(0.,-1.6,0.));
#11267=CARTESIAN_POINT('',(-0.18,-1.58,-2.20436423846524E-17));
#11268=CARTESIAN_POINT('Origin',(0.,-1.6,0.));
#11269=CARTESIAN_POINT('Origin',(0.0866025403784439,-0.4,-0.15));
#11270=CARTESIAN_POINT('',(0.173205080756888,-0.4,0.));
#11271=CARTESIAN_POINT('',(0.0866025403784439,-0.4,-0.15));
#11272=CARTESIAN_POINT('',(0.173205080756888,-0.4,0.));
#11273=CARTESIAN_POINT('',(0.0866025403784439,-0.64,-0.15));
#11274=CARTESIAN_POINT('',(0.0866025403784439,-0.4,-0.15));
#11275=CARTESIAN_POINT('',(0.173205080756888,-0.64,0.));
#11276=CARTESIAN_POINT('',(0.173205080756888,-0.64,0.));
#11277=CARTESIAN_POINT('',(0.173205080756888,-0.4,0.));
#11278=CARTESIAN_POINT('Origin',(-0.0866025403784438,-0.4,-0.15));
#11279=CARTESIAN_POINT('',(-0.0866025403784438,-0.4,-0.15));
#11280=CARTESIAN_POINT('',(0.0866025403784439,-0.4,-0.15));
#11281=CARTESIAN_POINT('',(-0.0866025403784438,-0.64,-0.15));
#11282=CARTESIAN_POINT('',(-0.0866025403784438,-0.4,-0.15));
#11283=CARTESIAN_POINT('',(0.0866025403784439,-0.64,-0.15));
#11284=CARTESIAN_POINT('Origin',(-0.173205080756888,-0.4,-2.77555756156289E-17));
#11285=CARTESIAN_POINT('',(-0.173205080756888,-0.4,-2.12115047744981E-17));
#11286=CARTESIAN_POINT('',(-0.0866025403784438,-0.4,-0.15));
#11287=CARTESIAN_POINT('',(-0.173205080756888,-0.64,-2.77555756156289E-17));
#11288=CARTESIAN_POINT('',(-0.173205080756888,-0.4,-2.12115047744981E-17));
#11289=CARTESIAN_POINT('',(-0.0866025403784438,-0.64,-0.15));
#11290=CARTESIAN_POINT('Origin',(-0.0866025403784439,-0.4,0.15));
#11291=CARTESIAN_POINT('',(-0.0866025403784439,-0.4,0.15));
#11292=CARTESIAN_POINT('',(-0.173205080756888,-0.4,-2.12115047744981E-17));
#11293=CARTESIAN_POINT('',(-0.0866025403784439,-0.64,0.15));
#11294=CARTESIAN_POINT('',(-0.0866025403784439,-0.4,0.15));
#11295=CARTESIAN_POINT('',(-0.173205080756888,-0.64,-2.12115047744981E-17));
#11296=CARTESIAN_POINT('Origin',(0.0866025403784439,-0.4,0.15));
#11297=CARTESIAN_POINT('',(0.0866025403784439,-0.4,0.15));
#11298=CARTESIAN_POINT('',(-0.0866025403784439,-0.4,0.15));
#11299=CARTESIAN_POINT('',(0.0866025403784439,-0.64,0.15));
#11300=CARTESIAN_POINT('',(0.0866025403784439,-0.4,0.15));
#11301=CARTESIAN_POINT('',(-0.0866025403784439,-0.64,0.15));
#11302=CARTESIAN_POINT('Origin',(0.173205080756888,-0.4,0.));
#11303=CARTESIAN_POINT('',(0.0866025403784439,-0.4,0.15));
#11304=CARTESIAN_POINT('',(0.0866025403784439,-0.64,0.15));
#11305=CARTESIAN_POINT('Origin',(0.,-0.4,-2.77555756156289E-17));
#11306=CARTESIAN_POINT('Origin',(0.,-0.64,-2.77555756156289E-17));
#11307=CARTESIAN_POINT('',(0.,0.,0.));
#11308=CARTESIAN_POINT('',(0.,0.,0.));
#11309=CARTESIAN_POINT('',(0.,0.,0.));
#11310=CARTESIAN_POINT('',(0.,0.,0.));
#11311=CARTESIAN_POINT('',(0.,0.,0.));
#11312=CARTESIAN_POINT('',(0.,0.,0.));
#11313=CARTESIAN_POINT('',(0.,0.,0.));
#11314=CARTESIAN_POINT('',(0.,0.,0.));
#11315=CARTESIAN_POINT('',(0.,0.,0.));
#11316=CARTESIAN_POINT('',(0.,0.,0.));
#11317=CARTESIAN_POINT('',(0.,0.,0.));
#11318=CARTESIAN_POINT('',(0.,0.,0.));
#11319=CARTESIAN_POINT('',(0.,0.,0.));
#11320=CARTESIAN_POINT('',(0.,0.,0.));
#11321=CARTESIAN_POINT('',(0.,0.,0.));
#11322=CARTESIAN_POINT('',(0.,0.,0.));
#11323=CARTESIAN_POINT('',(0.,0.,0.));
#11324=CARTESIAN_POINT('',(0.,0.,0.));
#11325=CARTESIAN_POINT('',(0.,0.,0.));
#11326=CARTESIAN_POINT('',(0.,0.,0.));
#11327=CARTESIAN_POINT('',(0.,0.,0.));
#11328=CARTESIAN_POINT('',(0.,0.,0.));
#11329=CARTESIAN_POINT('',(0.,0.,0.));
#11330=CARTESIAN_POINT('',(0.,0.,0.));
#11331=CARTESIAN_POINT('',(0.,0.,0.));
#11332=CARTESIAN_POINT('',(0.,0.,0.));
#11333=CARTESIAN_POINT('',(0.,0.,0.));
#11334=CARTESIAN_POINT('',(0.,0.,0.));
#11335=CARTESIAN_POINT('',(0.,0.,0.));
#11336=CARTESIAN_POINT('',(0.,0.,0.));
#11337=CARTESIAN_POINT('',(0.,0.,0.));
#11338=CARTESIAN_POINT('',(-4.5,-1.8,1.6));
#11339=CARTESIAN_POINT('',(-4.5,1.8,1.6));
#11340=CARTESIAN_POINT('',(4.5,-1.8,1.6));
#11341=CARTESIAN_POINT('',(4.5,1.8,1.6));
#11342=CARTESIAN_POINT('',(-4.8,-1.8,3.8));
#11343=CARTESIAN_POINT('',(-4.8,0.,3.8));
#11344=CARTESIAN_POINT('',(4.8,-1.8,3.8));
#11345=CARTESIAN_POINT('',(4.8,0.,3.8));
#11346=CARTESIAN_POINT('',(-3.75,-2.5,4.));
#11347=CARTESIAN_POINT('',(-1.25,-2.5,4.));
#11348=CARTESIAN_POINT('',(1.25,-2.5,4.));
#11349=CARTESIAN_POINT('',(3.75,-2.5,4.));
#11350=CARTESIAN_POINT('',(0.,0.,6.5));
#11351=CARTESIAN_POINT('',(2.75,0.,15.7));
#11352=CARTESIAN_POINT('',(0.,2.75,15.7));
#11353=CARTESIAN_POINT('',(-2.75,4.44089209850063E-16,15.7));
#11354=CARTESIAN_POINT('',(-8.88178419700125E-16,-2.75,15.7));
#11355=UNCERTAINTY_MEASURE_WITH_UNIT(LENGTH_MEASURE(0.001),#11433,
'DISTANCE_ACCURACY_VALUE',
'Maximum model space distance between geometric entities at asserted c
onnectivities');
#11356=UNCERTAINTY_MEASURE_WITH_UNIT(LENGTH_MEASURE(0.001),#11433,
'DISTANCE_ACCURACY_VALUE',
'Maximum model space distance between geometric entities at asserted c
onnectivities');
#11357=UNCERTAINTY_MEASURE_WITH_UNIT(LENGTH_MEASURE(0.001),#11433,
'DISTANCE_ACCURACY_VALUE',
'Maximum model space distance between geometric entities at asserted c
onnectivities');
#11358=UNCERTAINTY_MEASURE_WITH_UNIT(LENGTH_MEASURE(0.001),#11433,
'DISTANCE_ACCURACY_VALUE',
'Maximum model space distance between geometric entities at asserted c
onnectivities');
#11359=UNCERTAINTY_MEASURE_WITH_UNIT(LENGTH_MEASURE(0.001),#11433,
'DISTANCE_ACCURACY_VALUE',
'Maximum model space distance between geometric entities at asserted c
onnectivities');
#11360=UNCERTAINTY_MEASURE_WITH_UNIT(LENGTH_MEASURE(0.001),#11433,
'DISTANCE_ACCURACY_VALUE',
'Maximum model space distance between geometric entities at asserted c
onnectivities');
#11361=UNCERTAINTY_MEASURE_WITH_UNIT(LENGTH_MEASURE(0.001),#11433,
'DISTANCE_ACCURACY_VALUE',
'Maximum model space distance between geometric entities at asserted c
onnectivities');
#11362=UNCERTAINTY_MEASURE_WITH_UNIT(LENGTH_MEASURE(0.001),#11433,
'DISTANCE_ACCURACY_VALUE',
'Maximum model space distance between geometric entities at asserted c
onnectivities');
#11363=UNCERTAINTY_MEASURE_WITH_UNIT(LENGTH_MEASURE(0.001),#11433,
'DISTANCE_ACCURACY_VALUE',
'Maximum model space distance between geometric entities at asserted c
onnectivities');
#11364=UNCERTAINTY_MEASURE_WITH_UNIT(LENGTH_MEASURE(0.001),#11433,
'DISTANCE_ACCURACY_VALUE',
'Maximum model space distance between geometric entities at asserted c
onnectivities');
#11365=UNCERTAINTY_MEASURE_WITH_UNIT(LENGTH_MEASURE(0.001),#11433,
'DISTANCE_ACCURACY_VALUE',
'Maximum model space distance between geometric entities at asserted c
onnectivities');
#11366=UNCERTAINTY_MEASURE_WITH_UNIT(LENGTH_MEASURE(0.001),#11433,
'DISTANCE_ACCURACY_VALUE',
'Maximum model space distance between geometric entities at asserted c
onnectivities');
#11367=UNCERTAINTY_MEASURE_WITH_UNIT(LENGTH_MEASURE(0.001),#11433,
'DISTANCE_ACCURACY_VALUE',
'Maximum model space distance between geometric entities at asserted c
onnectivities');
#11368=UNCERTAINTY_MEASURE_WITH_UNIT(LENGTH_MEASURE(0.001),#11433,
'DISTANCE_ACCURACY_VALUE',
'Maximum model space distance between geometric entities at asserted c
onnectivities');
#11369=UNCERTAINTY_MEASURE_WITH_UNIT(LENGTH_MEASURE(0.001),#11433,
'DISTANCE_ACCURACY_VALUE',
'Maximum model space distance between geometric entities at asserted c
onnectivities');
#11370=UNCERTAINTY_MEASURE_WITH_UNIT(LENGTH_MEASURE(0.001),#11433,
'DISTANCE_ACCURACY_VALUE',
'Maximum model space distance between geometric entities at asserted c
onnectivities');
#11371=UNCERTAINTY_MEASURE_WITH_UNIT(LENGTH_MEASURE(0.001),#11433,
'DISTANCE_ACCURACY_VALUE',
'Maximum model space distance between geometric entities at asserted c
onnectivities');
#11372=UNCERTAINTY_MEASURE_WITH_UNIT(LENGTH_MEASURE(0.001),#11433,
'DISTANCE_ACCURACY_VALUE',
'Maximum model space distance between geometric entities at asserted c
onnectivities');
#11373=UNCERTAINTY_MEASURE_WITH_UNIT(LENGTH_MEASURE(0.001),#11433,
'DISTANCE_ACCURACY_VALUE',
'Maximum model space distance between geometric entities at asserted c
onnectivities');
#11374=UNCERTAINTY_MEASURE_WITH_UNIT(LENGTH_MEASURE(0.001),#11433,
'DISTANCE_ACCURACY_VALUE',
'Maximum model space distance between geometric entities at asserted c
onnectivities');
#11375=UNCERTAINTY_MEASURE_WITH_UNIT(LENGTH_MEASURE(0.001),#11433,
'DISTANCE_ACCURACY_VALUE',
'Maximum model space distance between geometric entities at asserted c
onnectivities');
#11376=UNCERTAINTY_MEASURE_WITH_UNIT(LENGTH_MEASURE(0.001),#11433,
'DISTANCE_ACCURACY_VALUE',
'Maximum model space distance between geometric entities at asserted c
onnectivities');
#11377=UNCERTAINTY_MEASURE_WITH_UNIT(LENGTH_MEASURE(0.001),#11433,
'DISTANCE_ACCURACY_VALUE',
'Maximum model space distance between geometric entities at asserted c
onnectivities');
#11378=UNCERTAINTY_MEASURE_WITH_UNIT(LENGTH_MEASURE(0.001),#11433,
'DISTANCE_ACCURACY_VALUE',
'Maximum model space distance between geometric entities at asserted c
onnectivities');
#11379=UNCERTAINTY_MEASURE_WITH_UNIT(LENGTH_MEASURE(0.001),#11433,
'DISTANCE_ACCURACY_VALUE',
'Maximum model space distance between geometric entities at asserted c
onnectivities');
#11380=UNCERTAINTY_MEASURE_WITH_UNIT(LENGTH_MEASURE(0.001),#11433,
'DISTANCE_ACCURACY_VALUE',
'Maximum model space distance between geometric entities at asserted c
onnectivities');
#11381=UNCERTAINTY_MEASURE_WITH_UNIT(LENGTH_MEASURE(0.001),#11433,
'DISTANCE_ACCURACY_VALUE',
'Maximum model space distance between geometric entities at asserted c
onnectivities');
#11382=UNCERTAINTY_MEASURE_WITH_UNIT(LENGTH_MEASURE(0.001),#11433,
'DISTANCE_ACCURACY_VALUE',
'Maximum model space distance between geometric entities at asserted c
onnectivities');
#11383=UNCERTAINTY_MEASURE_WITH_UNIT(LENGTH_MEASURE(0.001),#11433,
'DISTANCE_ACCURACY_VALUE',
'Maximum model space distance between geometric entities at asserted c
onnectivities');
#11384=UNCERTAINTY_MEASURE_WITH_UNIT(LENGTH_MEASURE(0.001),#11433,
'DISTANCE_ACCURACY_VALUE',
'Maximum model space distance between geometric entities at asserted c
onnectivities');
#11385=UNCERTAINTY_MEASURE_WITH_UNIT(LENGTH_MEASURE(0.001),#11433,
'DISTANCE_ACCURACY_VALUE',
'Maximum model space distance between geometric entities at asserted c
onnectivities');
#11386=UNCERTAINTY_MEASURE_WITH_UNIT(LENGTH_MEASURE(0.001),#11433,
'DISTANCE_ACCURACY_VALUE',
'Maximum model space distance between geometric entities at asserted c
onnectivities');
#11387=UNCERTAINTY_MEASURE_WITH_UNIT(LENGTH_MEASURE(0.001),#11433,
'DISTANCE_ACCURACY_VALUE',
'Maximum model space distance between geometric entities at asserted c
onnectivities');
#11388=UNCERTAINTY_MEASURE_WITH_UNIT(LENGTH_MEASURE(0.001),#11433,
'DISTANCE_ACCURACY_VALUE',
'Maximum model space distance between geometric entities at asserted c
onnectivities');
#11389=UNCERTAINTY_MEASURE_WITH_UNIT(LENGTH_MEASURE(0.001),#11433,
'DISTANCE_ACCURACY_VALUE',
'Maximum model space distance between geometric entities at asserted c
onnectivities');
#11390=UNCERTAINTY_MEASURE_WITH_UNIT(LENGTH_MEASURE(0.001),#11433,
'DISTANCE_ACCURACY_VALUE',
'Maximum model space distance between geometric entities at asserted c
onnectivities');
#11391=UNCERTAINTY_MEASURE_WITH_UNIT(LENGTH_MEASURE(0.001),#11433,
'DISTANCE_ACCURACY_VALUE',
'Maximum model space distance between geometric entities at asserted c
onnectivities');
#11392=UNCERTAINTY_MEASURE_WITH_UNIT(LENGTH_MEASURE(0.001),#11433,
'DISTANCE_ACCURACY_VALUE',
'Maximum model space distance between geometric entities at asserted c
onnectivities');
#11393=UNCERTAINTY_MEASURE_WITH_UNIT(LENGTH_MEASURE(0.001),#11433,
'DISTANCE_ACCURACY_VALUE',
'Maximum model space distance between geometric entities at asserted c
onnectivities');
#11394=(
GEOMETRIC_REPRESENTATION_CONTEXT(3)
GLOBAL_UNCERTAINTY_ASSIGNED_CONTEXT((#11355))
GLOBAL_UNIT_ASSIGNED_CONTEXT((#11433,#11435,#11436))
REPRESENTATION_CONTEXT('','3D')
);
#11395=(
GEOMETRIC_REPRESENTATION_CONTEXT(3)
GLOBAL_UNCERTAINTY_ASSIGNED_CONTEXT((#11356))
GLOBAL_UNIT_ASSIGNED_CONTEXT((#11433,#11435,#11436))
REPRESENTATION_CONTEXT('','3D')
);
#11396=(
GEOMETRIC_REPRESENTATION_CONTEXT(3)
GLOBAL_UNCERTAINTY_ASSIGNED_CONTEXT((#11357))
GLOBAL_UNIT_ASSIGNED_CONTEXT((#11433,#11435,#11436))
REPRESENTATION_CONTEXT('','3D')
);
#11397=(
GEOMETRIC_REPRESENTATION_CONTEXT(3)
GLOBAL_UNCERTAINTY_ASSIGNED_CONTEXT((#11358))
GLOBAL_UNIT_ASSIGNED_CONTEXT((#11433,#11435,#11436))
REPRESENTATION_CONTEXT('','3D')
);
#11398=(
GEOMETRIC_REPRESENTATION_CONTEXT(3)
GLOBAL_UNCERTAINTY_ASSIGNED_CONTEXT((#11359))
GLOBAL_UNIT_ASSIGNED_CONTEXT((#11433,#11435,#11436))
REPRESENTATION_CONTEXT('','3D')
);
#11399=(
GEOMETRIC_REPRESENTATION_CONTEXT(3)
GLOBAL_UNCERTAINTY_ASSIGNED_CONTEXT((#11360))
GLOBAL_UNIT_ASSIGNED_CONTEXT((#11433,#11435,#11436))
REPRESENTATION_CONTEXT('','3D')
);
#11400=(
GEOMETRIC_REPRESENTATION_CONTEXT(3)
GLOBAL_UNCERTAINTY_ASSIGNED_CONTEXT((#11361))
GLOBAL_UNIT_ASSIGNED_CONTEXT((#11433,#11435,#11436))
REPRESENTATION_CONTEXT('','3D')
);
#11401=(
GEOMETRIC_REPRESENTATION_CONTEXT(3)
GLOBAL_UNCERTAINTY_ASSIGNED_CONTEXT((#11362))
GLOBAL_UNIT_ASSIGNED_CONTEXT((#11433,#11435,#11436))
REPRESENTATION_CONTEXT('','3D')
);
#11402=(
GEOMETRIC_REPRESENTATION_CONTEXT(3)
GLOBAL_UNCERTAINTY_ASSIGNED_CONTEXT((#11363))
GLOBAL_UNIT_ASSIGNED_CONTEXT((#11433,#11435,#11436))
REPRESENTATION_CONTEXT('','3D')
);
#11403=(
GEOMETRIC_REPRESENTATION_CONTEXT(3)
GLOBAL_UNCERTAINTY_ASSIGNED_CONTEXT((#11364))
GLOBAL_UNIT_ASSIGNED_CONTEXT((#11433,#11435,#11436))
REPRESENTATION_CONTEXT('','3D')
);
#11404=(
GEOMETRIC_REPRESENTATION_CONTEXT(3)
GLOBAL_UNCERTAINTY_ASSIGNED_CONTEXT((#11365))
GLOBAL_UNIT_ASSIGNED_CONTEXT((#11433,#11435,#11436))
REPRESENTATION_CONTEXT('','3D')
);
#11405=(
GEOMETRIC_REPRESENTATION_CONTEXT(3)
GLOBAL_UNCERTAINTY_ASSIGNED_CONTEXT((#11366))
GLOBAL_UNIT_ASSIGNED_CONTEXT((#11433,#11435,#11436))
REPRESENTATION_CONTEXT('','3D')
);
#11406=(
GEOMETRIC_REPRESENTATION_CONTEXT(3)
GLOBAL_UNCERTAINTY_ASSIGNED_CONTEXT((#11367))
GLOBAL_UNIT_ASSIGNED_CONTEXT((#11433,#11435,#11436))
REPRESENTATION_CONTEXT('','3D')
);
#11407=(
GEOMETRIC_REPRESENTATION_CONTEXT(3)
GLOBAL_UNCERTAINTY_ASSIGNED_CONTEXT((#11368))
GLOBAL_UNIT_ASSIGNED_CONTEXT((#11433,#11435,#11436))
REPRESENTATION_CONTEXT('','3D')
);
#11408=(
GEOMETRIC_REPRESENTATION_CONTEXT(3)
GLOBAL_UNCERTAINTY_ASSIGNED_CONTEXT((#11369))
GLOBAL_UNIT_ASSIGNED_CONTEXT((#11433,#11435,#11436))
REPRESENTATION_CONTEXT('','3D')
);
#11409=(
GEOMETRIC_REPRESENTATION_CONTEXT(3)
GLOBAL_UNCERTAINTY_ASSIGNED_CONTEXT((#11370))
GLOBAL_UNIT_ASSIGNED_CONTEXT((#11433,#11435,#11436))
REPRESENTATION_CONTEXT('','3D')
);
#11410=(
GEOMETRIC_REPRESENTATION_CONTEXT(3)
GLOBAL_UNCERTAINTY_ASSIGNED_CONTEXT((#11371))
GLOBAL_UNIT_ASSIGNED_CONTEXT((#11433,#11435,#11436))
REPRESENTATION_CONTEXT('','3D')
);
#11411=(
GEOMETRIC_REPRESENTATION_CONTEXT(3)
GLOBAL_UNCERTAINTY_ASSIGNED_CONTEXT((#11372))
GLOBAL_UNIT_ASSIGNED_CONTEXT((#11433,#11435,#11436))
REPRESENTATION_CONTEXT('','3D')
);
#11412=(
GEOMETRIC_REPRESENTATION_CONTEXT(3)
GLOBAL_UNCERTAINTY_ASSIGNED_CONTEXT((#11373))
GLOBAL_UNIT_ASSIGNED_CONTEXT((#11433,#11435,#11436))
REPRESENTATION_CONTEXT('','3D')
);
#11413=(
GEOMETRIC_REPRESENTATION_CONTEXT(3)
GLOBAL_UNCERTAINTY_ASSIGNED_CONTEXT((#11374))
GLOBAL_UNIT_ASSIGNED_CONTEXT((#11433,#11435,#11436))
REPRESENTATION_CONTEXT('','3D')
);
#11414=(
GEOMETRIC_REPRESENTATION_CONTEXT(3)
GLOBAL_UNCERTAINTY_ASSIGNED_CONTEXT((#11375))
GLOBAL_UNIT_ASSIGNED_CONTEXT((#11433,#11435,#11436))
REPRESENTATION_CONTEXT('','3D')
);
#11415=(
GEOMETRIC_REPRESENTATION_CONTEXT(3)
GLOBAL_UNCERTAINTY_ASSIGNED_CONTEXT((#11376))
GLOBAL_UNIT_ASSIGNED_CONTEXT((#11433,#11435,#11436))
REPRESENTATION_CONTEXT('','3D')
);
#11416=(
GEOMETRIC_REPRESENTATION_CONTEXT(3)
GLOBAL_UNCERTAINTY_ASSIGNED_CONTEXT((#11377))
GLOBAL_UNIT_ASSIGNED_CONTEXT((#11433,#11435,#11436))
REPRESENTATION_CONTEXT('','3D')
);
#11417=(
GEOMETRIC_REPRESENTATION_CONTEXT(3)
GLOBAL_UNCERTAINTY_ASSIGNED_CONTEXT((#11378))
GLOBAL_UNIT_ASSIGNED_CONTEXT((#11433,#11435,#11436))
REPRESENTATION_CONTEXT('','3D')
);
#11418=(
GEOMETRIC_REPRESENTATION_CONTEXT(3)
GLOBAL_UNCERTAINTY_ASSIGNED_CONTEXT((#11379))
GLOBAL_UNIT_ASSIGNED_CONTEXT((#11433,#11435,#11436))
REPRESENTATION_CONTEXT('','3D')
);
#11419=(
GEOMETRIC_REPRESENTATION_CONTEXT(3)
GLOBAL_UNCERTAINTY_ASSIGNED_CONTEXT((#11380))
GLOBAL_UNIT_ASSIGNED_CONTEXT((#11433,#11435,#11436))
REPRESENTATION_CONTEXT('','3D')
);
#11420=(
GEOMETRIC_REPRESENTATION_CONTEXT(3)
GLOBAL_UNCERTAINTY_ASSIGNED_CONTEXT((#11381))
GLOBAL_UNIT_ASSIGNED_CONTEXT((#11433,#11435,#11436))
REPRESENTATION_CONTEXT('','3D')
);
#11421=(
GEOMETRIC_REPRESENTATION_CONTEXT(3)
GLOBAL_UNCERTAINTY_ASSIGNED_CONTEXT((#11382))
GLOBAL_UNIT_ASSIGNED_CONTEXT((#11433,#11435,#11436))
REPRESENTATION_CONTEXT('','3D')
);
#11422=(
GEOMETRIC_REPRESENTATION_CONTEXT(3)
GLOBAL_UNCERTAINTY_ASSIGNED_CONTEXT((#11383))
GLOBAL_UNIT_ASSIGNED_CONTEXT((#11433,#11435,#11436))
REPRESENTATION_CONTEXT('','3D')
);
#11423=(
GEOMETRIC_REPRESENTATION_CONTEXT(3)
GLOBAL_UNCERTAINTY_ASSIGNED_CONTEXT((#11384))
GLOBAL_UNIT_ASSIGNED_CONTEXT((#11433,#11435,#11436))
REPRESENTATION_CONTEXT('','3D')
);
#11424=(
GEOMETRIC_REPRESENTATION_CONTEXT(3)
GLOBAL_UNCERTAINTY_ASSIGNED_CONTEXT((#11385))
GLOBAL_UNIT_ASSIGNED_CONTEXT((#11433,#11435,#11436))
REPRESENTATION_CONTEXT('','3D')
);
#11425=(
GEOMETRIC_REPRESENTATION_CONTEXT(3)
GLOBAL_UNCERTAINTY_ASSIGNED_CONTEXT((#11386))
GLOBAL_UNIT_ASSIGNED_CONTEXT((#11433,#11435,#11436))
REPRESENTATION_CONTEXT('','3D')
);
#11426=(
GEOMETRIC_REPRESENTATION_CONTEXT(3)
GLOBAL_UNCERTAINTY_ASSIGNED_CONTEXT((#11387))
GLOBAL_UNIT_ASSIGNED_CONTEXT((#11433,#11435,#11436))
REPRESENTATION_CONTEXT('','3D')
);
#11427=(
GEOMETRIC_REPRESENTATION_CONTEXT(3)
GLOBAL_UNCERTAINTY_ASSIGNED_CONTEXT((#11388))
GLOBAL_UNIT_ASSIGNED_CONTEXT((#11433,#11435,#11436))
REPRESENTATION_CONTEXT('','3D')
);
#11428=(
GEOMETRIC_REPRESENTATION_CONTEXT(3)
GLOBAL_UNCERTAINTY_ASSIGNED_CONTEXT((#11389))
GLOBAL_UNIT_ASSIGNED_CONTEXT((#11433,#11435,#11436))
REPRESENTATION_CONTEXT('','3D')
);
#11429=(
GEOMETRIC_REPRESENTATION_CONTEXT(3)
GLOBAL_UNCERTAINTY_ASSIGNED_CONTEXT((#11390))
GLOBAL_UNIT_ASSIGNED_CONTEXT((#11433,#11435,#11436))
REPRESENTATION_CONTEXT('','3D')
);
#11430=(
GEOMETRIC_REPRESENTATION_CONTEXT(3)
GLOBAL_UNCERTAINTY_ASSIGNED_CONTEXT((#11391))
GLOBAL_UNIT_ASSIGNED_CONTEXT((#11433,#11435,#11436))
REPRESENTATION_CONTEXT('','3D')
);
#11431=(
GEOMETRIC_REPRESENTATION_CONTEXT(3)
GLOBAL_UNCERTAINTY_ASSIGNED_CONTEXT((#11392))
GLOBAL_UNIT_ASSIGNED_CONTEXT((#11433,#11435,#11436))
REPRESENTATION_CONTEXT('','3D')
);
#11432=(
GEOMETRIC_REPRESENTATION_CONTEXT(3)
GLOBAL_UNCERTAINTY_ASSIGNED_CONTEXT((#11393))
GLOBAL_UNIT_ASSIGNED_CONTEXT((#11433,#11435,#11436))
REPRESENTATION_CONTEXT('','3D')
);
#11433=(
LENGTH_UNIT()
NAMED_UNIT(*)
SI_UNIT(.CENTI.,.METRE.)
);
#11434=(
LENGTH_UNIT()
NAMED_UNIT(*)
SI_UNIT($,.METRE.)
);
#11435=(
NAMED_UNIT(*)
PLANE_ANGLE_UNIT()
SI_UNIT($,.RADIAN.)
);
#11436=(
NAMED_UNIT(*)
SI_UNIT($,.STERADIAN.)
SOLID_ANGLE_UNIT()
);
#11437=SHAPE_DEFINITION_REPRESENTATION(#11475,#11563);
#11438=SHAPE_DEFINITION_REPRESENTATION(#11476,#11564);
#11439=SHAPE_DEFINITION_REPRESENTATION(#11477,#11565);
#11440=SHAPE_DEFINITION_REPRESENTATION(#11478,#11566);
#11441=SHAPE_DEFINITION_REPRESENTATION(#11479,#11567);
#11442=SHAPE_DEFINITION_REPRESENTATION(#11480,#11568);
#11443=SHAPE_DEFINITION_REPRESENTATION(#11481,#11569);
#11444=SHAPE_DEFINITION_REPRESENTATION(#11482,#11570);
#11445=SHAPE_DEFINITION_REPRESENTATION(#11483,#11571);
#11446=SHAPE_DEFINITION_REPRESENTATION(#11484,#11572);
#11447=SHAPE_DEFINITION_REPRESENTATION(#11485,#11573);
#11448=SHAPE_DEFINITION_REPRESENTATION(#11486,#11574);
#11449=SHAPE_DEFINITION_REPRESENTATION(#11487,#11575);
#11450=SHAPE_DEFINITION_REPRESENTATION(#11488,#11576);
#11451=SHAPE_DEFINITION_REPRESENTATION(#11489,#11577);
#11452=SHAPE_DEFINITION_REPRESENTATION(#11490,#11578);
#11453=SHAPE_DEFINITION_REPRESENTATION(#11491,#11579);
#11454=SHAPE_DEFINITION_REPRESENTATION(#11492,#11580);
#11455=SHAPE_DEFINITION_REPRESENTATION(#11493,#11581);
#11456=SHAPE_DEFINITION_REPRESENTATION(#11494,#11582);
#11457=SHAPE_DEFINITION_REPRESENTATION(#11495,#11583);
#11458=SHAPE_DEFINITION_REPRESENTATION(#11496,#11584);
#11459=SHAPE_DEFINITION_REPRESENTATION(#11497,#11585);
#11460=SHAPE_DEFINITION_REPRESENTATION(#11498,#11586);
#11461=SHAPE_DEFINITION_REPRESENTATION(#11499,#11587);
#11462=SHAPE_DEFINITION_REPRESENTATION(#11500,#11588);
#11463=SHAPE_DEFINITION_REPRESENTATION(#11501,#11589);
#11464=SHAPE_DEFINITION_REPRESENTATION(#11502,#11590);
#11465=SHAPE_DEFINITION_REPRESENTATION(#11503,#11591);
#11466=SHAPE_DEFINITION_REPRESENTATION(#11504,#11592);
#11467=SHAPE_DEFINITION_REPRESENTATION(#11505,#11593);
#11468=SHAPE_DEFINITION_REPRESENTATION(#11506,#11594);
#11469=SHAPE_DEFINITION_REPRESENTATION(#11507,#11595);
#11470=SHAPE_DEFINITION_REPRESENTATION(#11508,#11596);
#11471=SHAPE_DEFINITION_REPRESENTATION(#11509,#11597);
#11472=SHAPE_DEFINITION_REPRESENTATION(#11510,#11598);
#11473=SHAPE_DEFINITION_REPRESENTATION(#11513,#11599);
#11474=SHAPE_DEFINITION_REPRESENTATION(#11514,#11600);
#11475=PRODUCT_DEFINITION_SHAPE('',$,#11602);
#11476=PRODUCT_DEFINITION_SHAPE('',$,#11603);
#11477=PRODUCT_DEFINITION_SHAPE('',$,#11604);
#11478=PRODUCT_DEFINITION_SHAPE('',$,#11605);
#11479=PRODUCT_DEFINITION_SHAPE('',$,#11606);
#11480=PRODUCT_DEFINITION_SHAPE('',$,#11607);
#11481=PRODUCT_DEFINITION_SHAPE('',$,#11608);
#11482=PRODUCT_DEFINITION_SHAPE('',$,#11609);
#11483=PRODUCT_DEFINITION_SHAPE('',$,#11610);
#11484=PRODUCT_DEFINITION_SHAPE('',$,#11611);
#11485=PRODUCT_DEFINITION_SHAPE('',$,#11612);
#11486=PRODUCT_DEFINITION_SHAPE('',$,#11613);
#11487=PRODUCT_DEFINITION_SHAPE('',$,#11614);
#11488=PRODUCT_DEFINITION_SHAPE('',$,#11615);
#11489=PRODUCT_DEFINITION_SHAPE('',$,#11616);
#11490=PRODUCT_DEFINITION_SHAPE('',$,#11617);
#11491=PRODUCT_DEFINITION_SHAPE('',$,#11618);
#11492=PRODUCT_DEFINITION_SHAPE('',$,#11619);
#11493=PRODUCT_DEFINITION_SHAPE('',$,#11620);
#11494=PRODUCT_DEFINITION_SHAPE('',$,#11621);
#11495=PRODUCT_DEFINITION_SHAPE('',$,#11622);
#11496=PRODUCT_DEFINITION_SHAPE('',$,#11623);
#11497=PRODUCT_DEFINITION_SHAPE('',$,#11624);
#11498=PRODUCT_DEFINITION_SHAPE('',$,#11625);
#11499=PRODUCT_DEFINITION_SHAPE('',$,#11626);
#11500=PRODUCT_DEFINITION_SHAPE('',$,#11627);
#11501=PRODUCT_DEFINITION_SHAPE('',$,#11628);
#11502=PRODUCT_DEFINITION_SHAPE('',$,#11629);
#11503=PRODUCT_DEFINITION_SHAPE('',$,#11630);
#11504=PRODUCT_DEFINITION_SHAPE('',$,#11631);
#11505=PRODUCT_DEFINITION_SHAPE('',$,#11632);
#11506=PRODUCT_DEFINITION_SHAPE('',$,#11633);
#11507=PRODUCT_DEFINITION_SHAPE('',$,#11634);
#11508=PRODUCT_DEFINITION_SHAPE('',$,#11635);
#11509=PRODUCT_DEFINITION_SHAPE('',$,#11636);
#11510=PRODUCT_DEFINITION_SHAPE('',$,#11637);
#11511=PRODUCT_DEFINITION_SHAPE($,$,#161);
#11512=PRODUCT_DEFINITION_SHAPE($,$,#162);
#11513=PRODUCT_DEFINITION_SHAPE('',$,#11638);
#11514=PRODUCT_DEFINITION_SHAPE('',$,#11639);
#11515=PRODUCT_DEFINITION_SHAPE($,$,#163);
#11516=PRODUCT_DEFINITION_SHAPE($,$,#164);
#11517=PRODUCT_DEFINITION_SHAPE($,$,#165);
#11518=PRODUCT_DEFINITION_SHAPE($,$,#166);
#11519=PRODUCT_DEFINITION_SHAPE($,$,#167);
#11520=PRODUCT_DEFINITION_SHAPE($,$,#168);
#11521=PRODUCT_DEFINITION_SHAPE($,$,#169);
#11522=PRODUCT_DEFINITION_SHAPE($,$,#170);
#11523=PRODUCT_DEFINITION_SHAPE($,$,#171);
#11524=PRODUCT_DEFINITION_SHAPE($,$,#172);
#11525=PRODUCT_DEFINITION_SHAPE($,$,#173);
#11526=PRODUCT_DEFINITION_SHAPE($,$,#174);
#11527=PRODUCT_DEFINITION_SHAPE($,$,#175);
#11528=PRODUCT_DEFINITION_SHAPE($,$,#176);
#11529=PRODUCT_DEFINITION_SHAPE($,$,#177);
#11530=PRODUCT_DEFINITION_SHAPE($,$,#178);
#11531=PRODUCT_DEFINITION_SHAPE($,$,#179);
#11532=PRODUCT_DEFINITION_SHAPE($,$,#180);
#11533=PRODUCT_DEFINITION_SHAPE($,$,#181);
#11534=PRODUCT_DEFINITION_SHAPE($,$,#182);
#11535=PRODUCT_DEFINITION_SHAPE($,$,#183);
#11536=PRODUCT_DEFINITION_SHAPE($,$,#184);
#11537=PRODUCT_DEFINITION_SHAPE($,$,#185);
#11538=PRODUCT_DEFINITION_SHAPE($,$,#186);
#11539=PRODUCT_DEFINITION_SHAPE($,$,#187);
#11540=PRODUCT_DEFINITION_SHAPE($,$,#188);
#11541=PRODUCT_DEFINITION_SHAPE($,$,#189);
#11542=PRODUCT_DEFINITION_SHAPE($,$,#190);
#11543=PRODUCT_DEFINITION_SHAPE($,$,#191);
#11544=PRODUCT_DEFINITION_SHAPE($,$,#192);
#11545=PRODUCT_DEFINITION_SHAPE($,$,#193);
#11546=PRODUCT_DEFINITION_SHAPE($,$,#194);
#11547=PRODUCT_DEFINITION_SHAPE($,$,#195);
#11548=PRODUCT_DEFINITION_SHAPE($,$,#196);
#11549=PRODUCT_DEFINITION_SHAPE($,$,#197);
#11550=PRODUCT_DEFINITION_SHAPE($,$,#198);
#11551=PRODUCT_DEFINITION_SHAPE($,$,#199);
#11552=PRODUCT_DEFINITION_SHAPE($,$,#200);
#11553=PRODUCT_DEFINITION_SHAPE($,$,#201);
#11554=PRODUCT_DEFINITION_SHAPE($,$,#202);
#11555=PRODUCT_DEFINITION_SHAPE($,$,#203);
#11556=PRODUCT_DEFINITION_SHAPE($,$,#204);
#11557=PRODUCT_DEFINITION_SHAPE($,$,#205);
#11558=PRODUCT_DEFINITION_SHAPE($,$,#206);
#11559=PRODUCT_DEFINITION_SHAPE($,$,#207);
#11560=PRODUCT_DEFINITION_SHAPE($,$,#208);
#11561=PRODUCT_DEFINITION_SHAPE($,$,#209);
#11562=PRODUCT_DEFINITION_SHAPE($,$,#210);
#11563=SHAPE_REPRESENTATION('',(#6502,#7211,#7212,#7213,#7214,#7215,#7216,
#7217,#7218,#7219,#7220,#7221,#7222,#7223,#7224,#7225,#7226,#7227,#7228,
#7229,#7230,#7231,#7232,#7233,#7234,#7235,#7236,#7237,#7238,#7239,#7240,
#7241,#7242,#7243,#7244,#7245,#7246,#7247,#7248,#7249,#7250,#7251,#7252,
#7253,#7254,#7255,#7256,#7257,#7258),#11394);
#11564=SHAPE_REPRESENTATION('',(#6503),#11395);
#11565=SHAPE_REPRESENTATION('',(#6522),#11396);
#11566=SHAPE_REPRESENTATION('',(#6547),#11397);
#11567=SHAPE_REPRESENTATION('',(#6572),#11398);
#11568=SHAPE_REPRESENTATION('',(#6692),#11399);
#11569=SHAPE_REPRESENTATION('',(#6701),#11400);
#11570=SHAPE_REPRESENTATION('',(#6715),#11401);
#11571=SHAPE_REPRESENTATION('',(#6724),#11402);
#11572=SHAPE_REPRESENTATION('',(#6733),#11403);
#11573=SHAPE_REPRESENTATION('',(#6747),#11404);
#11574=SHAPE_REPRESENTATION('',(#6756),#11405);
#11575=SHAPE_REPRESENTATION('',(#6765),#11406);
#11576=SHAPE_REPRESENTATION('',(#6779),#11407);
#11577=SHAPE_REPRESENTATION('',(#6788),#11408);
#11578=SHAPE_REPRESENTATION('',(#6797),#11409);
#11579=SHAPE_REPRESENTATION('',(#6811),#11410);
#11580=SHAPE_REPRESENTATION('',(#6820),#11411);
#11581=SHAPE_REPRESENTATION('',(#6826),#11412);
#11582=SHAPE_REPRESENTATION('',(#6832),#11413);
#11583=SHAPE_REPRESENTATION('',(#6887),#11414);
#11584=SHAPE_REPRESENTATION('',(#6910),#11415);
#11585=SHAPE_REPRESENTATION('',(#6929),#11416);
#11586=SHAPE_REPRESENTATION('',(#6952),#11417);
#11587=SHAPE_REPRESENTATION('',(#6970),#11418);
#11588=SHAPE_REPRESENTATION('',(#6988),#11419);
#11589=SHAPE_REPRESENTATION('',(#7006),#11420);
#11590=SHAPE_REPRESENTATION('',(#7024),#11421);
#11591=SHAPE_REPRESENTATION('',(#7045),#11422);
#11592=SHAPE_REPRESENTATION('',(#7066),#11423);
#11593=SHAPE_REPRESENTATION('',(#7079),#11424);
#11594=SHAPE_REPRESENTATION('',(#7086),#11425);
#11595=SHAPE_REPRESENTATION('',(#7093),#11426);
#11596=SHAPE_REPRESENTATION('',(#7117,#7159,#7160),#11427);
#11597=SHAPE_REPRESENTATION('',(#7118),#11428);
#11598=SHAPE_REPRESENTATION('',(#7146),#11429);
#11599=SHAPE_REPRESENTATION('',(#7161),#11430);
#11600=SHAPE_REPRESENTATION('',(#7185),#11431);
#11601=PRODUCT_DEFINITION_CONTEXT('part definition',#11717,'design');
#11602=PRODUCT_DEFINITION('PAT-072',
'PAT-072',#11640,#11601);
#11603=PRODUCT_DEFINITION('Base','Base',#11641,#11601);
#11604=PRODUCT_DEFINITION('Pedestal','Pedestal',#11642,#11601);
#11605=PRODUCT_DEFINITION('Pedestal (1)','Pedestal (1)',#11643,
#11601);
#11606=PRODUCT_DEFINITION('Distributor','Distributor',#11644,
#11601);
#11607=PRODUCT_DEFINITION('Outlet tube','Outlet tube',#11645,
#11601);
#11608=PRODUCT_DEFINITION('Metering plug','Metering plug',#11646,
#11601);
#11609=PRODUCT_DEFINITION('Metering stem gasket',
'Metering stem gasket',#11647,#11601);
#11610=PRODUCT_DEFINITION('Outlet tube (1)','Outlet tube (1)',
#11648,#11601);
#11611=PRODUCT_DEFINITION('Metering plug (1)',
'Metering plug (1)',#11649,#11601);
#11612=PRODUCT_DEFINITION('Metering stem gasket (1)',
'Metering stem gasket (1)',#11650,#11601);
#11613=PRODUCT_DEFINITION('Outlet tube (2)','Outlet tube (2)',
#11651,#11601);
#11614=PRODUCT_DEFINITION('Metering plug (2)',
'Metering plug (2)',#11652,#11601);
#11615=PRODUCT_DEFINITION('Metering stem gasket (2)',
'Metering stem gasket (2)',#11653,#11601);
#11616=PRODUCT_DEFINITION('Outlet tube (3)','Outlet tube (3)',#11654,
#11601);
#11617=PRODUCT_DEFINITION('Metering plug (3)',
'Metering plug (3)',#11655,#11601);
#11618=PRODUCT_DEFINITION('Metering stem gasket (3)',
'Metering stem gasket (3)',#11656,#11601);
#11619=PRODUCT_DEFINITION('Gallery closure','Gallery closure',
#11657,#11601);
#11620=PRODUCT_DEFINITION('Gallery closure (1)',
'Gallery closure (1)',#11658,#11601);
#11621=PRODUCT_DEFINITION('Reservoir','Reservoir',#11659,
#11601);
#11622=PRODUCT_DEFINITION('Sight glass gasket',
'Sight glass gasket',#11660,#11601);
#11623=PRODUCT_DEFINITION('Sight glass','Sight glass',#11661,
#11601);
#11624=PRODUCT_DEFINITION('Sight glass retainer',
'Sight glass retainer',#11662,#11601);
#11625=PRODUCT_DEFINITION('M2 sight screw','M2 sight screw',#11663,
#11601);
#11626=PRODUCT_DEFINITION('M2 sight screw (1)',
'M2 sight screw (1)',#11664,#11601);
#11627=PRODUCT_DEFINITION('M2 sight screw (2)',
'M2 sight screw (2)',#11665,#11601);
#11628=PRODUCT_DEFINITION('M2 sight screw (3)',
'M2 sight screw (3)',#11666,#11601);
#11629=PRODUCT_DEFINITION('Lid gasket','Lid gasket',#11667,
#11601);
#11630=PRODUCT_DEFINITION('Reservoir lid','Reservoir lid',#11668,
#11601);
#11631=PRODUCT_DEFINITION('Vented fill cap','Vented fill cap',#11669,
#11601);
#11632=PRODUCT_DEFINITION('Bonded foot','Bonded foot',#11670,
#11601);
#11633=PRODUCT_DEFINITION('Bonded foot (1)','Bonded foot (1)',
#11671,#11601);
#11634=PRODUCT_DEFINITION('M5x14 Cap Screw','M5x14 Cap Screw',
#11672,#11601);
#11635=PRODUCT_DEFINITION('Push-In Tube Fitting - 6 mm Tube, 1-8 Inch Tapered Pipe Thread',
'Push-In Tube Fitting - 6 mm Tube, 1-8 Inch Tapered Pipe Thread',#11673,
#11601);
#11636=PRODUCT_DEFINITION('Body','Body',#11674,#11601);
#11637=PRODUCT_DEFINITION('Release collar','Release collar',#11675,
#11601);
#11638=PRODUCT_DEFINITION('Hex Pipe Nipple - 1-4 Inch Tapered Pipe Thread',
'Hex Pipe Nipple - 1-4 Inch Tapered Pipe Thread',#11676,#11601);
#11639=PRODUCT_DEFINITION('Cap Screw - M4x16',
'Cap Screw - M4x16',#11677,#11601);
#11640=PRODUCT_DEFINITION_FORMATION('',$,#11719);
#11641=PRODUCT_DEFINITION_FORMATION('',$,#11720);
#11642=PRODUCT_DEFINITION_FORMATION('',$,#11721);
#11643=PRODUCT_DEFINITION_FORMATION('',$,#11722);
#11644=PRODUCT_DEFINITION_FORMATION('',$,#11723);
#11645=PRODUCT_DEFINITION_FORMATION('',$,#11724);
#11646=PRODUCT_DEFINITION_FORMATION('',$,#11725);
#11647=PRODUCT_DEFINITION_FORMATION('',$,#11726);
#11648=PRODUCT_DEFINITION_FORMATION('',$,#11727);
#11649=PRODUCT_DEFINITION_FORMATION('',$,#11728);
#11650=PRODUCT_DEFINITION_FORMATION('',$,#11729);
#11651=PRODUCT_DEFINITION_FORMATION('',$,#11730);
#11652=PRODUCT_DEFINITION_FORMATION('',$,#11731);
#11653=PRODUCT_DEFINITION_FORMATION('',$,#11732);
#11654=PRODUCT_DEFINITION_FORMATION('',$,#11733);
#11655=PRODUCT_DEFINITION_FORMATION('',$,#11734);
#11656=PRODUCT_DEFINITION_FORMATION('',$,#11735);
#11657=PRODUCT_DEFINITION_FORMATION('',$,#11736);
#11658=PRODUCT_DEFINITION_FORMATION('',$,#11737);
#11659=PRODUCT_DEFINITION_FORMATION('',$,#11738);
#11660=PRODUCT_DEFINITION_FORMATION('',$,#11739);
#11661=PRODUCT_DEFINITION_FORMATION('',$,#11740);
#11662=PRODUCT_DEFINITION_FORMATION('',$,#11741);
#11663=PRODUCT_DEFINITION_FORMATION('',$,#11742);
#11664=PRODUCT_DEFINITION_FORMATION('',$,#11743);
#11665=PRODUCT_DEFINITION_FORMATION('',$,#11744);
#11666=PRODUCT_DEFINITION_FORMATION('',$,#11745);
#11667=PRODUCT_DEFINITION_FORMATION('',$,#11746);
#11668=PRODUCT_DEFINITION_FORMATION('',$,#11747);
#11669=PRODUCT_DEFINITION_FORMATION('',$,#11748);
#11670=PRODUCT_DEFINITION_FORMATION('',$,#11749);
#11671=PRODUCT_DEFINITION_FORMATION('',$,#11750);
#11672=PRODUCT_DEFINITION_FORMATION('',$,#11751);
#11673=PRODUCT_DEFINITION_FORMATION('',$,#11752);
#11674=PRODUCT_DEFINITION_FORMATION('',$,#11753);
#11675=PRODUCT_DEFINITION_FORMATION('',$,#11754);
#11676=PRODUCT_DEFINITION_FORMATION('',$,#11755);
#11677=PRODUCT_DEFINITION_FORMATION('',$,#11756);
#11678=PRODUCT_RELATED_PRODUCT_CATEGORY('PAT-072',
'PAT-072',(#11719));
#11679=PRODUCT_RELATED_PRODUCT_CATEGORY('Base','Base',(#11720));
#11680=PRODUCT_RELATED_PRODUCT_CATEGORY('Pedestal','Pedestal',(#11721));
#11681=PRODUCT_RELATED_PRODUCT_CATEGORY('Pedestal (1)','Pedestal (1)',(#11722));
#11682=PRODUCT_RELATED_PRODUCT_CATEGORY('Distributor','Distributor',(#11723));
#11683=PRODUCT_RELATED_PRODUCT_CATEGORY('Outlet tube','Outlet tube',(#11724));
#11684=PRODUCT_RELATED_PRODUCT_CATEGORY('Metering plug','Metering plug',
(#11725));
#11685=PRODUCT_RELATED_PRODUCT_CATEGORY('Metering stem gasket',
'Metering stem gasket',(#11726));
#11686=PRODUCT_RELATED_PRODUCT_CATEGORY('Outlet tube (1)',
'Outlet tube (1)',(#11727));
#11687=PRODUCT_RELATED_PRODUCT_CATEGORY('Metering plug (1)',
'Metering plug (1)',(#11728));
#11688=PRODUCT_RELATED_PRODUCT_CATEGORY('Metering stem gasket (1)',
'Metering stem gasket (1)',(#11729));
#11689=PRODUCT_RELATED_PRODUCT_CATEGORY('Outlet tube (2)',
'Outlet tube (2)',(#11730));
#11690=PRODUCT_RELATED_PRODUCT_CATEGORY('Metering plug (2)',
'Metering plug (2)',(#11731));
#11691=PRODUCT_RELATED_PRODUCT_CATEGORY('Metering stem gasket (2)',
'Metering stem gasket (2)',(#11732));
#11692=PRODUCT_RELATED_PRODUCT_CATEGORY('Outlet tube (3)',
'Outlet tube (3)',(#11733));
#11693=PRODUCT_RELATED_PRODUCT_CATEGORY('Metering plug (3)',
'Metering plug (3)',(#11734));
#11694=PRODUCT_RELATED_PRODUCT_CATEGORY('Metering stem gasket (3)',
'Metering stem gasket (3)',(#11735));
#11695=PRODUCT_RELATED_PRODUCT_CATEGORY('Gallery closure',
'Gallery closure',(#11736));
#11696=PRODUCT_RELATED_PRODUCT_CATEGORY('Gallery closure (1)',
'Gallery closure (1)',(#11737));
#11697=PRODUCT_RELATED_PRODUCT_CATEGORY('Reservoir','Reservoir',(#11738));
#11698=PRODUCT_RELATED_PRODUCT_CATEGORY('Sight glass gasket',
'Sight glass gasket',(#11739));
#11699=PRODUCT_RELATED_PRODUCT_CATEGORY('Sight glass','Sight glass',(#11740));
#11700=PRODUCT_RELATED_PRODUCT_CATEGORY('Sight glass retainer',
'Sight glass retainer',(#11741));
#11701=PRODUCT_RELATED_PRODUCT_CATEGORY('M2 sight screw',
'M2 sight screw',(#11742));
#11702=PRODUCT_RELATED_PRODUCT_CATEGORY('M2 sight screw (1)',
'M2 sight screw (1)',(#11743));
#11703=PRODUCT_RELATED_PRODUCT_CATEGORY('M2 sight screw (2)',
'M2 sight screw (2)',(#11744));
#11704=PRODUCT_RELATED_PRODUCT_CATEGORY('M2 sight screw (3)',
'M2 sight screw (3)',(#11745));
#11705=PRODUCT_RELATED_PRODUCT_CATEGORY('Lid gasket','Lid gasket',(#11746));
#11706=PRODUCT_RELATED_PRODUCT_CATEGORY('Reservoir lid','Reservoir lid',
(#11747));
#11707=PRODUCT_RELATED_PRODUCT_CATEGORY('Vented fill cap',
'Vented fill cap',(#11748));
#11708=PRODUCT_RELATED_PRODUCT_CATEGORY('Bonded foot','Bonded foot',(#11749));
#11709=PRODUCT_RELATED_PRODUCT_CATEGORY('Bonded foot (1)',
'Bonded foot (1)',(#11750));
#11710=PRODUCT_RELATED_PRODUCT_CATEGORY('M5x14 Cap Screw',
'M5x14 Cap Screw',(#11751));
#11711=PRODUCT_RELATED_PRODUCT_CATEGORY(
'Push-In Tube Fitting - 6 mm Tube, 1-8 Inch Tapered Pipe Thread',
'Push-In Tube Fitting - 6 mm Tube, 1-8 Inch Tapered Pipe Thread',(#11752));
#11712=PRODUCT_RELATED_PRODUCT_CATEGORY('Body','Body',(#11753));
#11713=PRODUCT_RELATED_PRODUCT_CATEGORY('Release collar',
'Release collar',(#11754));
#11714=PRODUCT_RELATED_PRODUCT_CATEGORY(
'Hex Pipe Nipple - 1-4 Inch Tapered Pipe Thread',
'Hex Pipe Nipple - 1-4 Inch Tapered Pipe Thread',(#11755));
#11715=PRODUCT_RELATED_PRODUCT_CATEGORY('Cap Screw - M4x16',
'Cap Screw - M4x16',(#11756));
#11716=APPLICATION_PROTOCOL_DEFINITION('international standard',
'automotive_design',2009,#11717);
#11717=APPLICATION_CONTEXT(
'Core Data for Automotive Mechanical Design Process');
#11718=PRODUCT_CONTEXT('part definition',#11717,'mechanical');
#11719=PRODUCT('PAT-072','PAT-072',
'PAT-072',(#11718));
#11720=PRODUCT('Base','Base','Base',(#11718));
#11721=PRODUCT('Pedestal','Pedestal','Pedestal',(#11718));
#11722=PRODUCT('Pedestal (1)','Pedestal (1)','Pedestal (1)',(#11718));
#11723=PRODUCT('Distributor','Distributor','Distributor',
(#11718));
#11724=PRODUCT('Outlet tube','Outlet tube','Outlet tube',(#11718));
#11725=PRODUCT('Metering plug','Metering plug',
'Metering plug',(#11718));
#11726=PRODUCT('Metering stem gasket','Metering stem gasket',
'Metering stem gasket',(#11718));
#11727=PRODUCT('Outlet tube (1)','Outlet tube (1)',
'Outlet tube (1)',(#11718));
#11728=PRODUCT('Metering plug (1)','Metering plug (1)',
'Metering plug (1)',(#11718));
#11729=PRODUCT('Metering stem gasket (1)','Metering stem gasket (1)',
'Metering stem gasket (1)',(#11718));
#11730=PRODUCT('Outlet tube (2)','Outlet tube (2)',
'Outlet tube (2)',(#11718));
#11731=PRODUCT('Metering plug (2)','Metering plug (2)',
'Metering plug (2)',(#11718));
#11732=PRODUCT('Metering stem gasket (2)','Metering stem gasket (2)',
'Metering stem gasket (2)',(#11718));
#11733=PRODUCT('Outlet tube (3)','Outlet tube (3)',
'Outlet tube (3)',(#11718));
#11734=PRODUCT('Metering plug (3)','Metering plug (3)',
'Metering plug (3)',(#11718));
#11735=PRODUCT('Metering stem gasket (3)','Metering stem gasket (3)',
'Metering stem gasket (3)',(#11718));
#11736=PRODUCT('Gallery closure','Gallery closure',
'Gallery closure',(#11718));
#11737=PRODUCT('Gallery closure (1)','Gallery closure (1)',
'Gallery closure (1)',(#11718));
#11738=PRODUCT('Reservoir','Reservoir','Reservoir',(#11718));
#11739=PRODUCT('Sight glass gasket','Sight glass gasket',
'Sight glass gasket',(#11718));
#11740=PRODUCT('Sight glass','Sight glass','Sight glass',(#11718));
#11741=PRODUCT('Sight glass retainer','Sight glass retainer',
'Sight glass retainer',(#11718));
#11742=PRODUCT('M2 sight screw','M2 sight screw',
'M2 sight screw',(#11718));
#11743=PRODUCT('M2 sight screw (1)','M2 sight screw (1)',
'M2 sight screw (1)',(#11718));
#11744=PRODUCT('M2 sight screw (2)','M2 sight screw (2)',
'M2 sight screw (2)',(#11718));
#11745=PRODUCT('M2 sight screw (3)','M2 sight screw (3)',
'M2 sight screw (3)',(#11718));
#11746=PRODUCT('Lid gasket','Lid gasket','Lid gasket',(#11718));
#11747=PRODUCT('Reservoir lid','Reservoir lid',
'Reservoir lid',(#11718));
#11748=PRODUCT('Vented fill cap','Vented fill cap',
'Vented fill cap',(#11718));
#11749=PRODUCT('Bonded foot','Bonded foot','Bonded foot',
(#11718));
#11750=PRODUCT('Bonded foot (1)','Bonded foot (1)',
'Bonded foot (1)',(#11718));
#11751=PRODUCT('M5x14 Cap Screw','M5x14 Cap Screw',
'M5x14 Cap Screw',(#11718));
#11752=PRODUCT('Push-In Tube Fitting - 6 mm Tube, 1-8 Inch Tapered Pipe Thread',
'Push-In Tube Fitting - 6 mm Tube, 1-8 Inch Tapered Pipe Thread',
'Push-In Tube Fitting - 6 mm Tube, 1-8 Inch Tapered Pipe Thread',(#11718));
#11753=PRODUCT('Body','Body','Body',(#11718));
#11754=PRODUCT('Release collar','Release collar',
'Release collar',(#11718));
#11755=PRODUCT('Hex Pipe Nipple - 1-4 Inch Tapered Pipe Thread',
'Hex Pipe Nipple - 1-4 Inch Tapered Pipe Thread',
'Hex Pipe Nipple - 1-4 Inch Tapered Pipe Thread',(#11718));
#11756=PRODUCT('Cap Screw - M4x16','Cap Screw - M4x16',
'Cap Screw - M4x16',(#11718));
#11757=PRESENTATION_STYLE_ASSIGNMENT((#11762));
#11758=PRESENTATION_STYLE_ASSIGNMENT((#11763));
#11759=PRESENTATION_STYLE_ASSIGNMENT((#11764));
#11760=PRESENTATION_STYLE_ASSIGNMENT((#11765));
#11761=PRESENTATION_STYLE_ASSIGNMENT((#11766));
#11762=SURFACE_STYLE_USAGE(.BOTH.,#11767);
#11763=SURFACE_STYLE_USAGE(.BOTH.,#11768);
#11764=SURFACE_STYLE_USAGE(.BOTH.,#11769);
#11765=SURFACE_STYLE_USAGE(.BOTH.,#11770);
#11766=SURFACE_STYLE_USAGE(.BOTH.,#11771);
#11767=SURFACE_SIDE_STYLE('',(#11772));
#11768=SURFACE_SIDE_STYLE('',(#11773));
#11769=SURFACE_SIDE_STYLE('',(#11774));
#11770=SURFACE_SIDE_STYLE('',(#11775));
#11771=SURFACE_SIDE_STYLE('',(#11776));
#11772=SURFACE_STYLE_FILL_AREA(#11777);
#11773=SURFACE_STYLE_FILL_AREA(#11778);
#11774=SURFACE_STYLE_FILL_AREA(#11779);
#11775=SURFACE_STYLE_FILL_AREA(#11780);
#11776=SURFACE_STYLE_FILL_AREA(#11781);
#11777=FILL_AREA_STYLE('Steel - Satin',(#11782));
#11778=FILL_AREA_STYLE('CAD Library Painted - Deep blue',(#11783));
#11779=FILL_AREA_STYLE('CAD Library Painted - Engineering blue',(#11784));
#11780=FILL_AREA_STYLE('CAD Library Painted - Steel gray',(#11785));
#11781=FILL_AREA_STYLE('CAD Library Painted - Graphite',(#11786));
#11782=FILL_AREA_STYLE_COLOUR('Steel - Satin',#11787);
#11783=FILL_AREA_STYLE_COLOUR('CAD Library Painted - Deep blue',#11788);
#11784=FILL_AREA_STYLE_COLOUR('CAD Library Painted - Engineering blue',
#11789);
#11785=FILL_AREA_STYLE_COLOUR('CAD Library Painted - Steel gray',#11790);
#11786=FILL_AREA_STYLE_COLOUR('CAD Library Painted - Graphite',#11791);
#11787=COLOUR_RGB('Steel - Satin',0.627450980392157,0.627450980392157,0.627450980392157);
#11788=COLOUR_RGB('CAD Library Painted - Deep blue',0.0784313725490196,
0.203921568627451,0.349019607843137);
#11789=COLOUR_RGB('CAD Library Painted - Engineering blue',0.12156862745098,
0.356862745098039,0.6);
#11790=COLOUR_RGB('CAD Library Painted - Steel gray',0.592156862745098,
0.631372549019608,0.67843137254902);
#11791=COLOUR_RGB('CAD Library Painted - Graphite',0.168627450980392,0.192156862745098,
0.231372549019608);
#11792=COLOUR_RGB('Dark Blue',0.08,0.2,0.34);
#11793=FILL_AREA_STYLE_COLOUR('',#11792);
#11794=FILL_AREA_STYLE('',(#11793));
#11795=SURFACE_STYLE_FILL_AREA(#11794);
#11796=SURFACE_SIDE_STYLE('',(#11795));
#11797=SURFACE_STYLE_USAGE(.BOTH.,#11796);
#11798=PRESENTATION_STYLE_ASSIGNMENT((#11797));
#11799=COLOUR_RGB('Light Blue',0.38,0.62,0.78);
#11800=FILL_AREA_STYLE_COLOUR('',#11799);
#11801=FILL_AREA_STYLE('',(#11800));
#11802=SURFACE_STYLE_FILL_AREA(#11801);
#11803=SURFACE_SIDE_STYLE('',(#11802));
#11804=SURFACE_STYLE_USAGE(.BOTH.,#11803);
#11805=PRESENTATION_STYLE_ASSIGNMENT((#11804));
#11806=COLOUR_RGB('Sky Blue',0.24,0.69,0.87);
#11807=FILL_AREA_STYLE_COLOUR('',#11806);
#11808=FILL_AREA_STYLE('',(#11807));
#11809=SURFACE_STYLE_FILL_AREA(#11808);
#11810=SURFACE_SIDE_STYLE('',(#11809));
#11811=SURFACE_STYLE_USAGE(.BOTH.,#11810);
#11812=PRESENTATION_STYLE_ASSIGNMENT((#11811));
#11813=COLOUR_RGB('Grey',0.48,0.52,0.57);
#11814=FILL_AREA_STYLE_COLOUR('',#11813);
#11815=FILL_AREA_STYLE('',(#11814));
#11816=SURFACE_STYLE_FILL_AREA(#11815);
#11817=SURFACE_SIDE_STYLE('',(#11816));
#11818=SURFACE_STYLE_USAGE(.BOTH.,#11817);
#11819=PRESENTATION_STYLE_ASSIGNMENT((#11818));
#11820=COLOUR_RGB('Black',0.12,0.14,0.17);
#11821=FILL_AREA_STYLE_COLOUR('',#11820);
#11822=FILL_AREA_STYLE('',(#11821));
#11823=SURFACE_STYLE_FILL_AREA(#11822);
#11824=SURFACE_SIDE_STYLE('',(#11823));
#11825=SURFACE_STYLE_USAGE(.BOTH.,#11824);
#11826=PRESENTATION_STYLE_ASSIGNMENT((#11825));
#11827=COLOUR_RGB('Off White',0.89,0.88,0.83);
#11828=FILL_AREA_STYLE_COLOUR('',#11827);
#11829=FILL_AREA_STYLE('',(#11828));
#11830=SURFACE_STYLE_FILL_AREA(#11829);
#11831=SURFACE_SIDE_STYLE('',(#11830));
#11832=SURFACE_STYLE_USAGE(.BOTH.,#11831);
#11833=PRESENTATION_STYLE_ASSIGNMENT((#11832));
ENDSEC;
END-ISO-10303-21;
